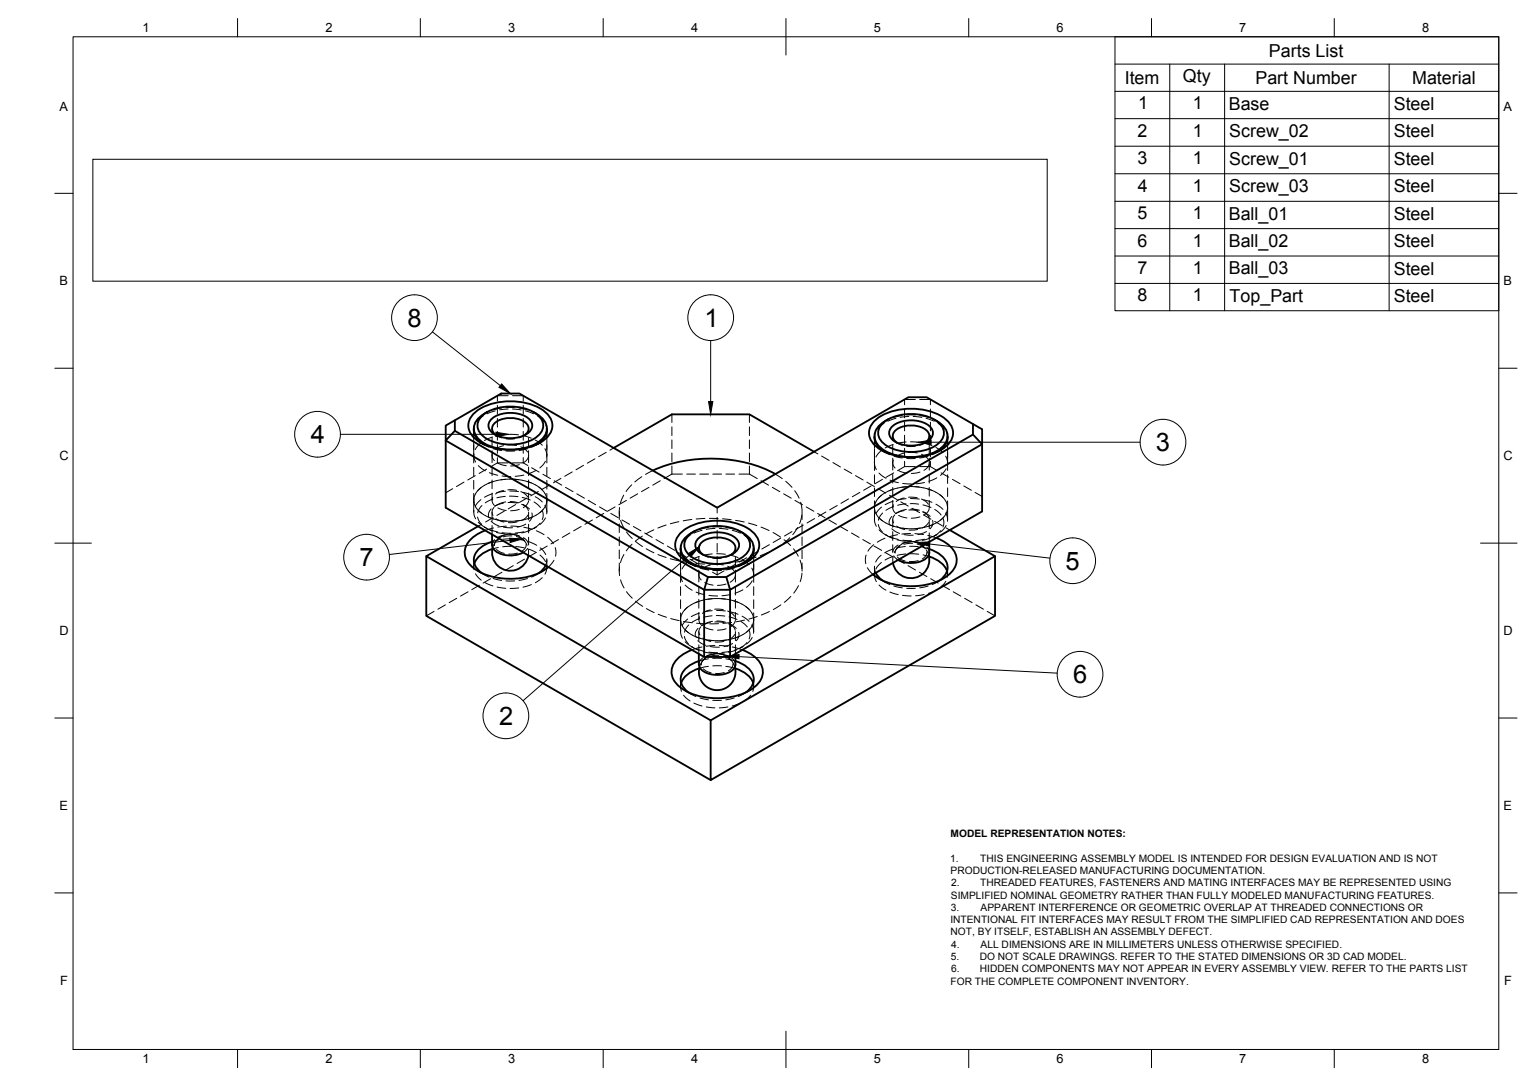
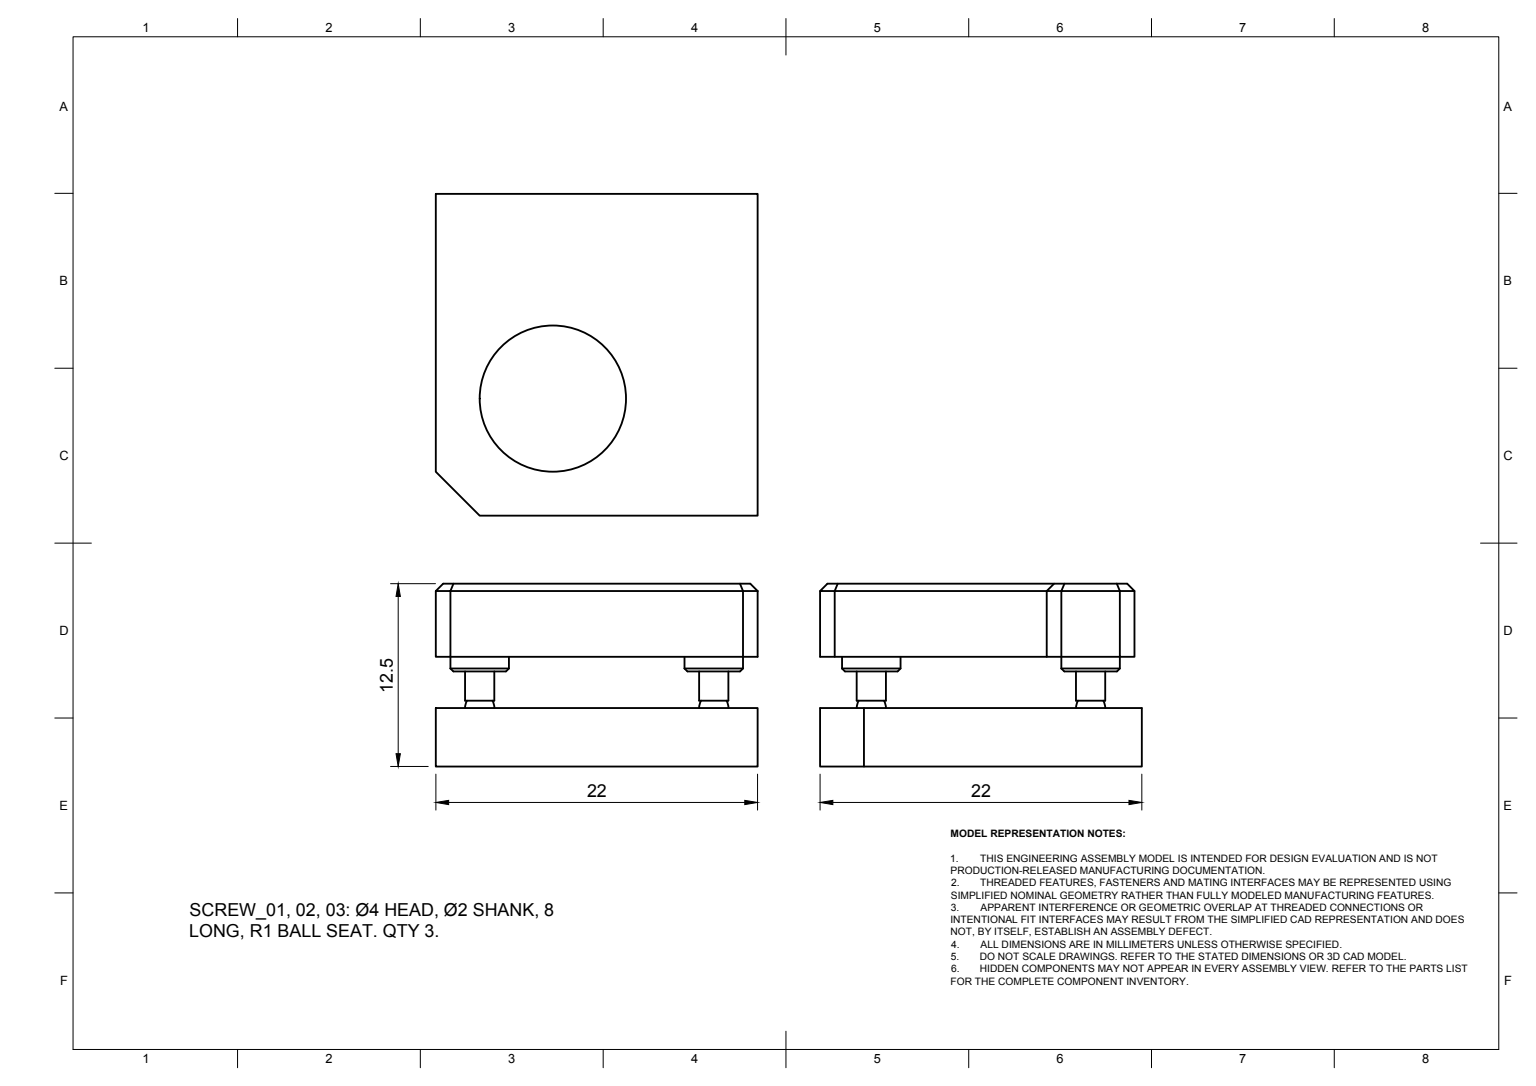
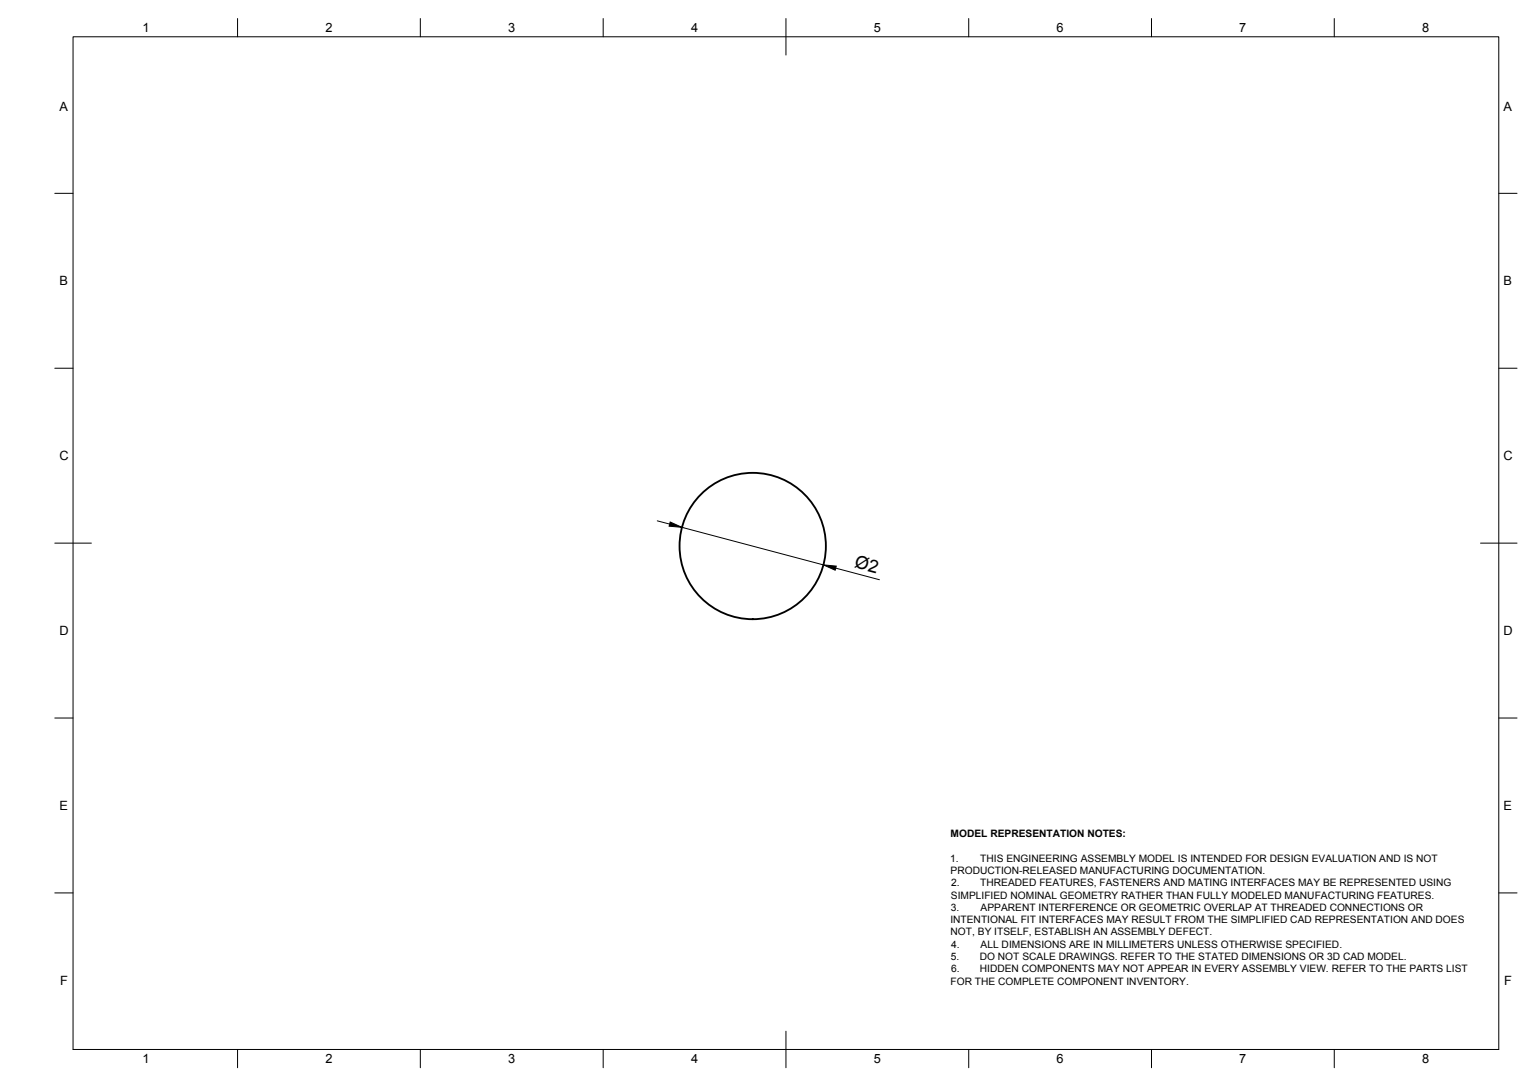
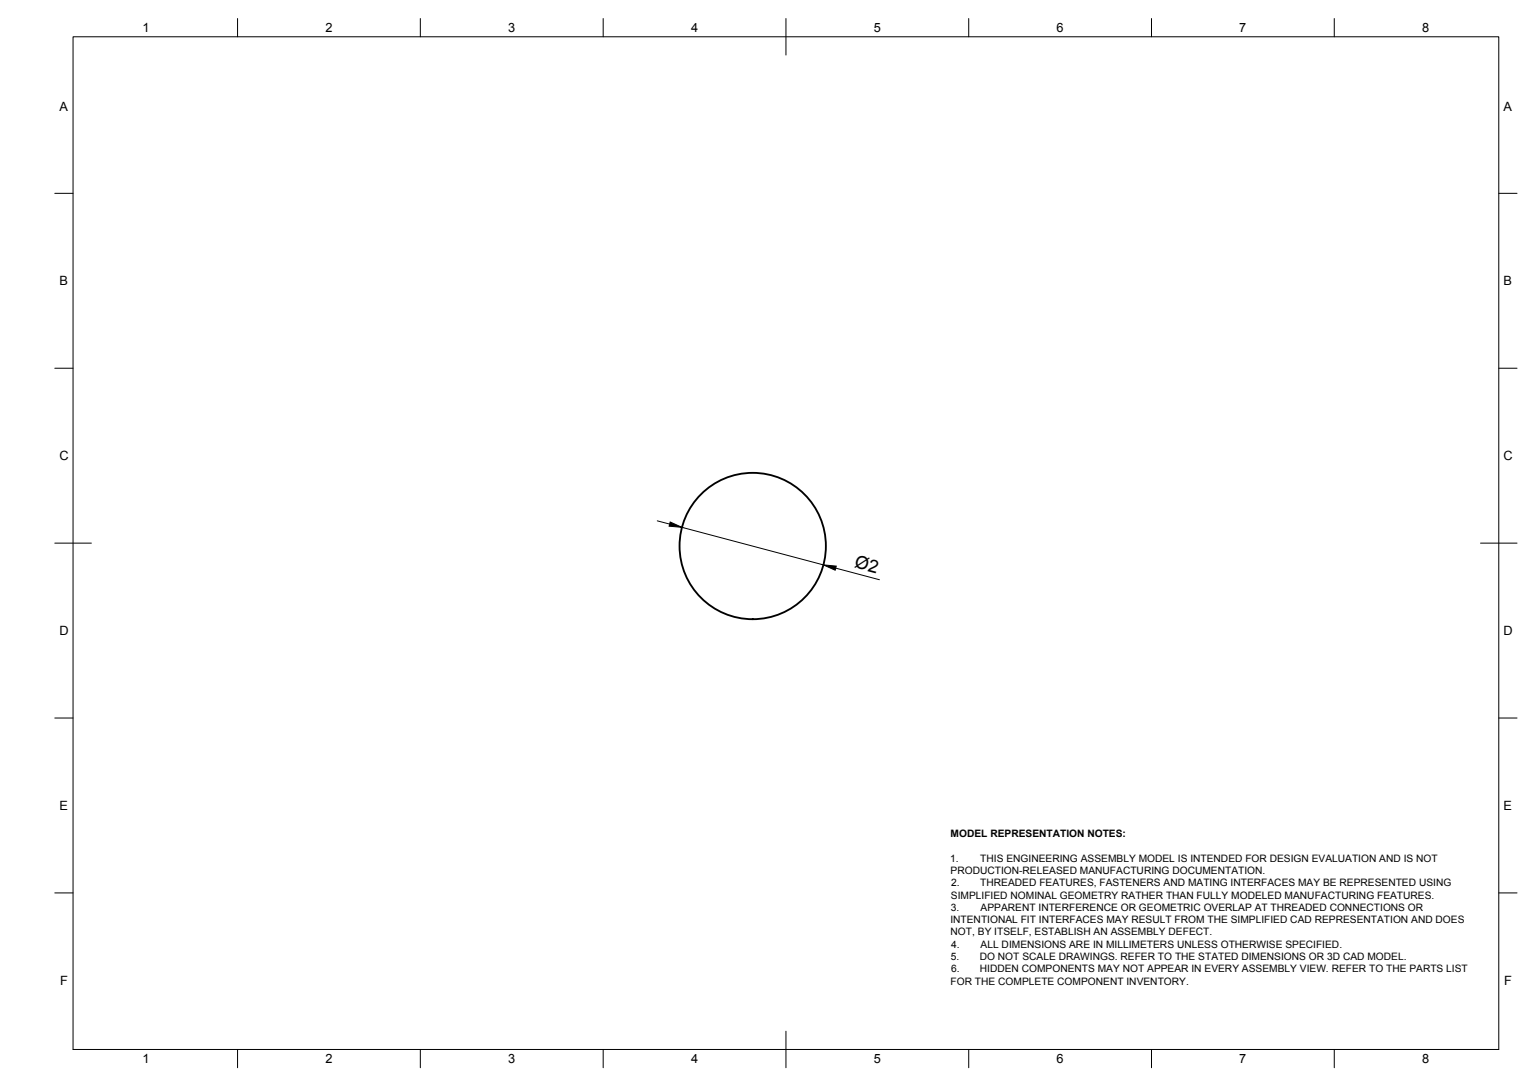
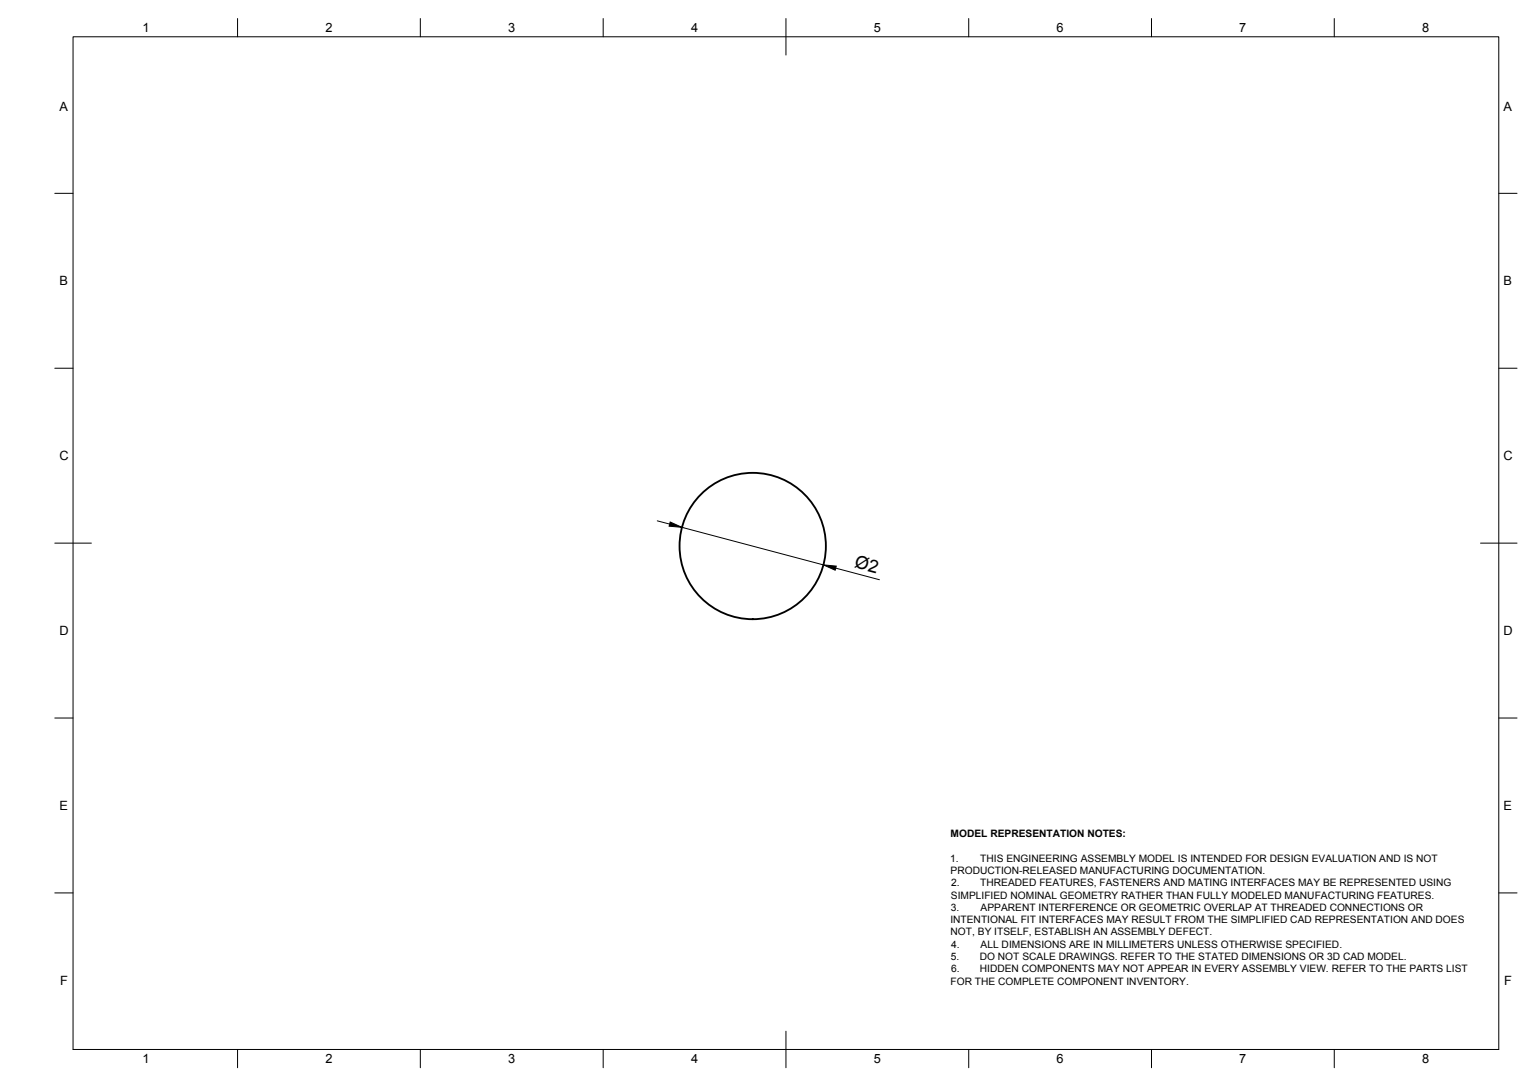
ISO-10303-21;
HEADER;
/* Generated by software containing ST-Developer
 * from STEP Tools, Inc. (www.steptools.com) 
 */

FILE_DESCRIPTION(
/* description */ (''),
/* implementation_level */ '2;1');

FILE_NAME(
/* name */ 'BR-151',
/* time_stamp */ '2026-10-04T23:23:09-07:00',
/* author */ (''),
/* organization */ (''),
/* preprocessor_version */ 'ST-DEVELOPER v20.2',
/* originating_system */ 'Autodesk Translation Framework v15.15.0.0',
/* authorisation */ '');

FILE_SCHEMA (('AUTOMOTIVE_DESIGN { 1 0 10303 214 3 1 1 }'));
ENDSEC;

DATA;
#10=MECHANICAL_DESIGN_GEOMETRIC_PRESENTATION_REPRESENTATION('',(#65,#66,
#67,#68,#69,#70,#71,#72,#73,#74,#75),#2676);
#11=ITEM_DEFINED_TRANSFORMATION($,$,#1577,#1754);
#12=ITEM_DEFINED_TRANSFORMATION($,$,#1606,#1755);
#13=ITEM_DEFINED_TRANSFORMATION($,$,#1639,#1756);
#14=ITEM_DEFINED_TRANSFORMATION($,$,#1672,#1757);
#15=ITEM_DEFINED_TRANSFORMATION($,$,#1705,#1758);
#16=ITEM_DEFINED_TRANSFORMATION($,$,#1708,#1759);
#17=ITEM_DEFINED_TRANSFORMATION($,$,#1711,#1760);
#18=ITEM_DEFINED_TRANSFORMATION($,$,#1714,#1761);
#19=(
REPRESENTATION_RELATIONSHIP($,$,#2708,#2707)
REPRESENTATION_RELATIONSHIP_WITH_TRANSFORMATION(#11)
SHAPE_REPRESENTATION_RELATIONSHIP()
);
#20=(
REPRESENTATION_RELATIONSHIP($,$,#2709,#2707)
REPRESENTATION_RELATIONSHIP_WITH_TRANSFORMATION(#12)
SHAPE_REPRESENTATION_RELATIONSHIP()
);
#21=(
REPRESENTATION_RELATIONSHIP($,$,#2710,#2707)
REPRESENTATION_RELATIONSHIP_WITH_TRANSFORMATION(#13)
SHAPE_REPRESENTATION_RELATIONSHIP()
);
#22=(
REPRESENTATION_RELATIONSHIP($,$,#2711,#2707)
REPRESENTATION_RELATIONSHIP_WITH_TRANSFORMATION(#14)
SHAPE_REPRESENTATION_RELATIONSHIP()
);
#23=(
REPRESENTATION_RELATIONSHIP($,$,#2712,#2707)
REPRESENTATION_RELATIONSHIP_WITH_TRANSFORMATION(#15)
SHAPE_REPRESENTATION_RELATIONSHIP()
);
#24=(
REPRESENTATION_RELATIONSHIP($,$,#2713,#2707)
REPRESENTATION_RELATIONSHIP_WITH_TRANSFORMATION(#16)
SHAPE_REPRESENTATION_RELATIONSHIP()
);
#25=(
REPRESENTATION_RELATIONSHIP($,$,#2714,#2707)
REPRESENTATION_RELATIONSHIP_WITH_TRANSFORMATION(#17)
SHAPE_REPRESENTATION_RELATIONSHIP()
);
#26=(
REPRESENTATION_RELATIONSHIP($,$,#2715,#2707)
REPRESENTATION_RELATIONSHIP_WITH_TRANSFORMATION(#18)
SHAPE_REPRESENTATION_RELATIONSHIP()
);
#27=CONTEXT_DEPENDENT_SHAPE_REPRESENTATION(#19,#2699);
#28=CONTEXT_DEPENDENT_SHAPE_REPRESENTATION(#20,#2700);
#29=CONTEXT_DEPENDENT_SHAPE_REPRESENTATION(#21,#2701);
#30=CONTEXT_DEPENDENT_SHAPE_REPRESENTATION(#22,#2702);
#31=CONTEXT_DEPENDENT_SHAPE_REPRESENTATION(#23,#2703);
#32=CONTEXT_DEPENDENT_SHAPE_REPRESENTATION(#24,#2704);
#33=CONTEXT_DEPENDENT_SHAPE_REPRESENTATION(#25,#2705);
#34=CONTEXT_DEPENDENT_SHAPE_REPRESENTATION(#26,#2706);
#35=NEXT_ASSEMBLY_USAGE_OCCURRENCE('Base:1','Base:1','Base:1',#2717,#2718,
'Base:1');
#36=NEXT_ASSEMBLY_USAGE_OCCURRENCE('Screw_02:1','Screw_02:1',
'Screw_02:1',#2717,#2719,'Screw_02:1');
#37=NEXT_ASSEMBLY_USAGE_OCCURRENCE('Screw_01:1','Screw_01:1',
'Screw_01:1',#2717,#2720,'Screw_01:1');
#38=NEXT_ASSEMBLY_USAGE_OCCURRENCE('Screw_03:1','Screw_03:1',
'Screw_03:1',#2717,#2721,'Screw_03:1');
#39=NEXT_ASSEMBLY_USAGE_OCCURRENCE('Ball_01:1','Ball_01:1','Ball_01:1',
#2717,#2722,'Ball_01:1');
#40=NEXT_ASSEMBLY_USAGE_OCCURRENCE('Ball_02:1','Ball_02:1','Ball_02:1',
#2717,#2723,'Ball_02:1');
#41=NEXT_ASSEMBLY_USAGE_OCCURRENCE('Ball_03:1','Ball_03:1','Ball_03:1',
#2717,#2724,'Ball_03:1');
#42=NEXT_ASSEMBLY_USAGE_OCCURRENCE('Top_part:1','Top_part:1',
'Top_part:1',#2717,#2725,'Top_part:1');
#43=SPHERICAL_SURFACE('',#1637,1.);
#44=SPHERICAL_SURFACE('',#1670,1.);
#45=SPHERICAL_SURFACE('',#1703,1.);
#46=SPHERICAL_SURFACE('',#1706,1.);
#47=SPHERICAL_SURFACE('',#1709,1.);
#48=SPHERICAL_SURFACE('',#1712,1.);
#49=SHAPE_REPRESENTATION_RELATIONSHIP('SRR','None',#2708,#57);
#50=SHAPE_REPRESENTATION_RELATIONSHIP('SRR','None',#2709,#58);
#51=SHAPE_REPRESENTATION_RELATIONSHIP('SRR','None',#2710,#59);
#52=SHAPE_REPRESENTATION_RELATIONSHIP('SRR','None',#2711,#60);
#53=SHAPE_REPRESENTATION_RELATIONSHIP('SRR','None',#2712,#61);
#54=SHAPE_REPRESENTATION_RELATIONSHIP('SRR','None',#2713,#62);
#55=SHAPE_REPRESENTATION_RELATIONSHIP('SRR','None',#2714,#63);
#56=SHAPE_REPRESENTATION_RELATIONSHIP('SRR','None',#2715,#64);
#57=ADVANCED_BREP_SHAPE_REPRESENTATION('',(#76),#2668);
#58=ADVANCED_BREP_SHAPE_REPRESENTATION('',(#77,#78),#2669);
#59=ADVANCED_BREP_SHAPE_REPRESENTATION('',(#79,#80),#2670);
#60=ADVANCED_BREP_SHAPE_REPRESENTATION('',(#81,#82),#2671);
#61=ADVANCED_BREP_SHAPE_REPRESENTATION('',(#83),#2672);
#62=ADVANCED_BREP_SHAPE_REPRESENTATION('',(#84),#2673);
#63=ADVANCED_BREP_SHAPE_REPRESENTATION('',(#85),#2674);
#64=ADVANCED_BREP_SHAPE_REPRESENTATION('',(#86),#2675);
#65=STYLED_ITEM('',(#2757),#76);
#66=STYLED_ITEM('',(#2757),#77);
#67=STYLED_ITEM('',(#2757),#78);
#68=STYLED_ITEM('',(#2757),#79);
#69=STYLED_ITEM('',(#2757),#80);
#70=STYLED_ITEM('',(#2757),#81);
#71=STYLED_ITEM('',(#2757),#82);
#72=STYLED_ITEM('',(#2757),#83);
#73=STYLED_ITEM('',(#2757),#84);
#74=STYLED_ITEM('',(#2757),#85);
#75=STYLED_ITEM('',(#2757),#86);
#76=MANIFOLD_SOLID_BREP('Body1',#1476);
#77=MANIFOLD_SOLID_BREP('Body1',#1477);
#78=MANIFOLD_SOLID_BREP('Body1',#1478);
#79=MANIFOLD_SOLID_BREP('Body1',#1479);
#80=MANIFOLD_SOLID_BREP('Body1',#1480);
#81=MANIFOLD_SOLID_BREP('Body1',#1481);
#82=MANIFOLD_SOLID_BREP('Body1',#1482);
#83=MANIFOLD_SOLID_BREP('Body1',#1483);
#84=MANIFOLD_SOLID_BREP('Body1',#1484);
#85=MANIFOLD_SOLID_BREP('Body1',#1485);
#86=MANIFOLD_SOLID_BREP('Body1',#1486);
#87=CYLINDRICAL_SURFACE('',#1585,2.);
#88=CYLINDRICAL_SURFACE('',#1589,2.);
#89=CYLINDRICAL_SURFACE('',#1593,2.);
#90=CYLINDRICAL_SURFACE('',#1598,5.);
#91=CYLINDRICAL_SURFACE('',#1610,1.);
#92=CYLINDRICAL_SURFACE('',#1614,2.);
#93=CYLINDRICAL_SURFACE('',#1622,1.);
#94=CYLINDRICAL_SURFACE('',#1626,1.);
#95=CYLINDRICAL_SURFACE('',#1630,2.);
#96=CYLINDRICAL_SURFACE('',#1643,1.);
#97=CYLINDRICAL_SURFACE('',#1647,2.);
#98=CYLINDRICAL_SURFACE('',#1655,1.);
#99=CYLINDRICAL_SURFACE('',#1659,1.);
#100=CYLINDRICAL_SURFACE('',#1663,2.);
#101=CYLINDRICAL_SURFACE('',#1676,1.);
#102=CYLINDRICAL_SURFACE('',#1680,2.);
#103=CYLINDRICAL_SURFACE('',#1688,1.);
#104=CYLINDRICAL_SURFACE('',#1692,1.);
#105=CYLINDRICAL_SURFACE('',#1696,2.);
#106=CYLINDRICAL_SURFACE('',#1721,2.);
#107=CYLINDRICAL_SURFACE('',#1725,2.);
#108=CYLINDRICAL_SURFACE('',#1753,2.);
#109=FACE_BOUND('',#287,.T.);
#110=FACE_BOUND('',#288,.T.);
#111=FACE_BOUND('',#289,.T.);
#112=FACE_BOUND('',#290,.T.);
#113=FACE_BOUND('',#306,.T.);
#114=FACE_BOUND('',#308,.T.);
#115=FACE_BOUND('',#313,.T.);
#116=FACE_BOUND('',#316,.T.);
#117=FACE_BOUND('',#321,.T.);
#118=FACE_BOUND('',#325,.T.);
#119=FACE_BOUND('',#329,.T.);
#120=FACE_BOUND('',#334,.T.);
#121=FACE_BOUND('',#337,.T.);
#122=FACE_BOUND('',#342,.T.);
#123=FACE_BOUND('',#346,.T.);
#124=FACE_BOUND('',#350,.T.);
#125=FACE_BOUND('',#355,.T.);
#126=FACE_BOUND('',#358,.T.);
#127=FACE_BOUND('',#363,.T.);
#128=FACE_BOUND('',#367,.T.);
#129=FACE_BOUND('',#375,.T.);
#130=FACE_BOUND('',#376,.T.);
#131=FACE_BOUND('',#377,.T.);
#132=FACE_BOUND('',#390,.T.);
#133=FACE_BOUND('',#391,.T.);
#134=FACE_BOUND('',#392,.T.);
#135=PLANE('',#1581);
#136=PLANE('',#1595);
#137=PLANE('',#1596);
#138=PLANE('',#1597);
#139=PLANE('',#1600);
#140=PLANE('',#1601);
#141=PLANE('',#1602);
#142=PLANE('',#1603);
#143=PLANE('',#1604);
#144=PLANE('',#1605);
#145=PLANE('',#1607);
#146=PLANE('',#1616);
#147=PLANE('',#1619);
#148=PLANE('',#1624);
#149=PLANE('',#1628);
#150=PLANE('',#1634);
#151=PLANE('',#1640);
#152=PLANE('',#1649);
#153=PLANE('',#1652);
#154=PLANE('',#1657);
#155=PLANE('',#1661);
#156=PLANE('',#1667);
#157=PLANE('',#1673);
#158=PLANE('',#1682);
#159=PLANE('',#1685);
#160=PLANE('',#1690);
#161=PLANE('',#1694);
#162=PLANE('',#1700);
#163=PLANE('',#1718);
#164=PLANE('',#1727);
#165=PLANE('',#1728);
#166=PLANE('',#1729);
#167=PLANE('',#1730);
#168=PLANE('',#1731);
#169=PLANE('',#1732);
#170=PLANE('',#1733);
#171=PLANE('',#1734);
#172=PLANE('',#1735);
#173=PLANE('',#1737);
#174=PLANE('',#1738);
#175=PLANE('',#1739);
#176=PLANE('',#1740);
#177=PLANE('',#1741);
#178=PLANE('',#1742);
#179=PLANE('',#1743);
#180=PLANE('',#1744);
#181=PLANE('',#1745);
#182=PLANE('',#1746);
#183=PLANE('',#1747);
#184=PLANE('',#1748);
#185=PLANE('',#1749);
#186=PLANE('',#1750);
#187=FACE_OUTER_BOUND('',#285,.T.);
#188=FACE_OUTER_BOUND('',#286,.T.);
#189=FACE_OUTER_BOUND('',#291,.T.);
#190=FACE_OUTER_BOUND('',#292,.T.);
#191=FACE_OUTER_BOUND('',#293,.T.);
#192=FACE_OUTER_BOUND('',#294,.T.);
#193=FACE_OUTER_BOUND('',#295,.T.);
#194=FACE_OUTER_BOUND('',#296,.T.);
#195=FACE_OUTER_BOUND('',#297,.T.);
#196=FACE_OUTER_BOUND('',#298,.T.);
#197=FACE_OUTER_BOUND('',#299,.T.);
#198=FACE_OUTER_BOUND('',#300,.T.);
#199=FACE_OUTER_BOUND('',#301,.T.);
#200=FACE_OUTER_BOUND('',#302,.T.);
#201=FACE_OUTER_BOUND('',#303,.T.);
#202=FACE_OUTER_BOUND('',#304,.T.);
#203=FACE_OUTER_BOUND('',#305,.T.);
#204=FACE_OUTER_BOUND('',#307,.T.);
#205=FACE_OUTER_BOUND('',#309,.T.);
#206=FACE_OUTER_BOUND('',#310,.T.);
#207=FACE_OUTER_BOUND('',#311,.T.);
#208=FACE_OUTER_BOUND('',#312,.T.);
#209=FACE_OUTER_BOUND('',#314,.T.);
#210=FACE_OUTER_BOUND('',#315,.T.);
#211=FACE_OUTER_BOUND('',#317,.T.);
#212=FACE_OUTER_BOUND('',#318,.T.);
#213=FACE_OUTER_BOUND('',#319,.T.);
#214=FACE_OUTER_BOUND('',#320,.T.);
#215=FACE_OUTER_BOUND('',#322,.T.);
#216=FACE_OUTER_BOUND('',#323,.T.);
#217=FACE_OUTER_BOUND('',#324,.T.);
#218=FACE_OUTER_BOUND('',#326,.T.);
#219=FACE_OUTER_BOUND('',#327,.T.);
#220=FACE_OUTER_BOUND('',#328,.T.);
#221=FACE_OUTER_BOUND('',#330,.T.);
#222=FACE_OUTER_BOUND('',#331,.T.);
#223=FACE_OUTER_BOUND('',#332,.T.);
#224=FACE_OUTER_BOUND('',#333,.T.);
#225=FACE_OUTER_BOUND('',#335,.T.);
#226=FACE_OUTER_BOUND('',#336,.T.);
#227=FACE_OUTER_BOUND('',#338,.T.);
#228=FACE_OUTER_BOUND('',#339,.T.);
#229=FACE_OUTER_BOUND('',#340,.T.);
#230=FACE_OUTER_BOUND('',#341,.T.);
#231=FACE_OUTER_BOUND('',#343,.T.);
#232=FACE_OUTER_BOUND('',#344,.T.);
#233=FACE_OUTER_BOUND('',#345,.T.);
#234=FACE_OUTER_BOUND('',#347,.T.);
#235=FACE_OUTER_BOUND('',#348,.T.);
#236=FACE_OUTER_BOUND('',#349,.T.);
#237=FACE_OUTER_BOUND('',#351,.T.);
#238=FACE_OUTER_BOUND('',#352,.T.);
#239=FACE_OUTER_BOUND('',#353,.T.);
#240=FACE_OUTER_BOUND('',#354,.T.);
#241=FACE_OUTER_BOUND('',#356,.T.);
#242=FACE_OUTER_BOUND('',#357,.T.);
#243=FACE_OUTER_BOUND('',#359,.T.);
#244=FACE_OUTER_BOUND('',#360,.T.);
#245=FACE_OUTER_BOUND('',#361,.T.);
#246=FACE_OUTER_BOUND('',#362,.T.);
#247=FACE_OUTER_BOUND('',#364,.T.);
#248=FACE_OUTER_BOUND('',#365,.T.);
#249=FACE_OUTER_BOUND('',#366,.T.);
#250=FACE_OUTER_BOUND('',#368,.T.);
#251=FACE_OUTER_BOUND('',#369,.T.);
#252=FACE_OUTER_BOUND('',#370,.T.);
#253=FACE_OUTER_BOUND('',#371,.T.);
#254=FACE_OUTER_BOUND('',#372,.T.);
#255=FACE_OUTER_BOUND('',#373,.T.);
#256=FACE_OUTER_BOUND('',#374,.T.);
#257=FACE_OUTER_BOUND('',#378,.T.);
#258=FACE_OUTER_BOUND('',#379,.T.);
#259=FACE_OUTER_BOUND('',#380,.T.);
#260=FACE_OUTER_BOUND('',#381,.T.);
#261=FACE_OUTER_BOUND('',#382,.T.);
#262=FACE_OUTER_BOUND('',#383,.T.);
#263=FACE_OUTER_BOUND('',#384,.T.);
#264=FACE_OUTER_BOUND('',#385,.T.);
#265=FACE_OUTER_BOUND('',#386,.T.);
#266=FACE_OUTER_BOUND('',#387,.T.);
#267=FACE_OUTER_BOUND('',#388,.T.);
#268=FACE_OUTER_BOUND('',#389,.T.);
#269=FACE_OUTER_BOUND('',#393,.T.);
#270=FACE_OUTER_BOUND('',#394,.T.);
#271=FACE_OUTER_BOUND('',#395,.T.);
#272=FACE_OUTER_BOUND('',#396,.T.);
#273=FACE_OUTER_BOUND('',#397,.T.);
#274=FACE_OUTER_BOUND('',#398,.T.);
#275=FACE_OUTER_BOUND('',#399,.T.);
#276=FACE_OUTER_BOUND('',#400,.T.);
#277=FACE_OUTER_BOUND('',#401,.T.);
#278=FACE_OUTER_BOUND('',#402,.T.);
#279=FACE_OUTER_BOUND('',#403,.T.);
#280=FACE_OUTER_BOUND('',#404,.T.);
#281=FACE_OUTER_BOUND('',#405,.T.);
#282=FACE_OUTER_BOUND('',#406,.T.);
#283=FACE_OUTER_BOUND('',#407,.T.);
#284=FACE_OUTER_BOUND('',#408,.T.);
#285=EDGE_LOOP('',(#998,#999,#1000,#1001));
#286=EDGE_LOOP('',(#1002,#1003,#1004,#1005,#1006));
#287=EDGE_LOOP('',(#1007));
#288=EDGE_LOOP('',(#1008));
#289=EDGE_LOOP('',(#1009));
#290=EDGE_LOOP('',(#1010));
#291=EDGE_LOOP('',(#1011,#1012,#1013,#1014));
#292=EDGE_LOOP('',(#1015,#1016,#1017,#1018));
#293=EDGE_LOOP('',(#1019,#1020,#1021,#1022));
#294=EDGE_LOOP('',(#1023,#1024,#1025,#1026));
#295=EDGE_LOOP('',(#1027,#1028,#1029,#1030));
#296=EDGE_LOOP('',(#1031));
#297=EDGE_LOOP('',(#1032));
#298=EDGE_LOOP('',(#1033));
#299=EDGE_LOOP('',(#1034,#1035,#1036,#1037));
#300=EDGE_LOOP('',(#1038,#1039,#1040,#1041));
#301=EDGE_LOOP('',(#1042,#1043,#1044,#1045));
#302=EDGE_LOOP('',(#1046,#1047,#1048,#1049));
#303=EDGE_LOOP('',(#1050,#1051,#1052,#1053));
#304=EDGE_LOOP('',(#1054,#1055,#1056,#1057));
#305=EDGE_LOOP('',(#1058,#1059,#1060,#1061,#1062));
#306=EDGE_LOOP('',(#1063));
#307=EDGE_LOOP('',(#1064));
#308=EDGE_LOOP('',(#1065));
#309=EDGE_LOOP('',(#1066,#1067,#1068,#1069));
#310=EDGE_LOOP('',(#1070,#1071,#1072,#1073));
#311=EDGE_LOOP('',(#1074,#1075,#1076,#1077));
#312=EDGE_LOOP('',(#1078));
#313=EDGE_LOOP('',(#1079));
#314=EDGE_LOOP('',(#1080,#1081,#1082,#1083));
#315=EDGE_LOOP('',(#1084));
#316=EDGE_LOOP('',(#1085));
#317=EDGE_LOOP('',(#1086,#1087,#1088,#1089));
#318=EDGE_LOOP('',(#1090));
#319=EDGE_LOOP('',(#1091,#1092,#1093,#1094));
#320=EDGE_LOOP('',(#1095));
#321=EDGE_LOOP('',(#1096));
#322=EDGE_LOOP('',(#1097,#1098,#1099,#1100));
#323=EDGE_LOOP('',(#1101,#1102,#1103,#1104));
#324=EDGE_LOOP('',(#1105));
#325=EDGE_LOOP('',(#1106));
#326=EDGE_LOOP('',(#1107,#1108,#1109,#1110));
#327=EDGE_LOOP('',(#1111,#1112,#1113));
#328=EDGE_LOOP('',(#1114));
#329=EDGE_LOOP('',(#1115));
#330=EDGE_LOOP('',(#1116,#1117,#1118,#1119));
#331=EDGE_LOOP('',(#1120,#1121,#1122,#1123));
#332=EDGE_LOOP('',(#1124,#1125,#1126,#1127));
#333=EDGE_LOOP('',(#1128));
#334=EDGE_LOOP('',(#1129));
#335=EDGE_LOOP('',(#1130,#1131,#1132,#1133));
#336=EDGE_LOOP('',(#1134));
#337=EDGE_LOOP('',(#1135));
#338=EDGE_LOOP('',(#1136,#1137,#1138,#1139));
#339=EDGE_LOOP('',(#1140));
#340=EDGE_LOOP('',(#1141,#1142,#1143,#1144));
#341=EDGE_LOOP('',(#1145));
#342=EDGE_LOOP('',(#1146));
#343=EDGE_LOOP('',(#1147,#1148,#1149,#1150));
#344=EDGE_LOOP('',(#1151,#1152,#1153,#1154));
#345=EDGE_LOOP('',(#1155));
#346=EDGE_LOOP('',(#1156));
#347=EDGE_LOOP('',(#1157,#1158,#1159,#1160));
#348=EDGE_LOOP('',(#1161,#1162,#1163));
#349=EDGE_LOOP('',(#1164));
#350=EDGE_LOOP('',(#1165));
#351=EDGE_LOOP('',(#1166,#1167,#1168,#1169));
#352=EDGE_LOOP('',(#1170,#1171,#1172,#1173));
#353=EDGE_LOOP('',(#1174,#1175,#1176,#1177));
#354=EDGE_LOOP('',(#1178));
#355=EDGE_LOOP('',(#1179));
#356=EDGE_LOOP('',(#1180,#1181,#1182,#1183));
#357=EDGE_LOOP('',(#1184));
#358=EDGE_LOOP('',(#1185));
#359=EDGE_LOOP('',(#1186,#1187,#1188,#1189));
#360=EDGE_LOOP('',(#1190));
#361=EDGE_LOOP('',(#1191,#1192,#1193,#1194));
#362=EDGE_LOOP('',(#1195));
#363=EDGE_LOOP('',(#1196));
#364=EDGE_LOOP('',(#1197,#1198,#1199,#1200));
#365=EDGE_LOOP('',(#1201,#1202,#1203,#1204));
#366=EDGE_LOOP('',(#1205));
#367=EDGE_LOOP('',(#1206));
#368=EDGE_LOOP('',(#1207,#1208,#1209,#1210));
#369=EDGE_LOOP('',(#1211,#1212,#1213));
#370=EDGE_LOOP('',(#1214,#1215));
#371=EDGE_LOOP('',(#1216,#1217));
#372=EDGE_LOOP('',(#1218,#1219));
#373=EDGE_LOOP('',(#1220,#1221,#1222,#1223));
#374=EDGE_LOOP('',(#1224,#1225,#1226,#1227,#1228,#1229,#1230,#1231,#1232,
#1233,#1234));
#375=EDGE_LOOP('',(#1235));
#376=EDGE_LOOP('',(#1236));
#377=EDGE_LOOP('',(#1237));
#378=EDGE_LOOP('',(#1238,#1239,#1240,#1241));
#379=EDGE_LOOP('',(#1242,#1243,#1244,#1245));
#380=EDGE_LOOP('',(#1246,#1247,#1248,#1249));
#381=EDGE_LOOP('',(#1250,#1251,#1252,#1253));
#382=EDGE_LOOP('',(#1254,#1255,#1256,#1257));
#383=EDGE_LOOP('',(#1258,#1259,#1260,#1261));
#384=EDGE_LOOP('',(#1262,#1263,#1264,#1265));
#385=EDGE_LOOP('',(#1266,#1267,#1268,#1269));
#386=EDGE_LOOP('',(#1270,#1271,#1272,#1273));
#387=EDGE_LOOP('',(#1274,#1275,#1276,#1277));
#388=EDGE_LOOP('',(#1278,#1279,#1280,#1281));
#389=EDGE_LOOP('',(#1282,#1283,#1284,#1285,#1286,#1287,#1288,#1289,#1290,
#1291,#1292));
#390=EDGE_LOOP('',(#1293));
#391=EDGE_LOOP('',(#1294));
#392=EDGE_LOOP('',(#1295));
#393=EDGE_LOOP('',(#1296,#1297,#1298,#1299));
#394=EDGE_LOOP('',(#1300,#1301,#1302,#1303));
#395=EDGE_LOOP('',(#1304,#1305,#1306,#1307));
#396=EDGE_LOOP('',(#1308,#1309,#1310,#1311));
#397=EDGE_LOOP('',(#1312,#1313,#1314,#1315));
#398=EDGE_LOOP('',(#1316,#1317,#1318,#1319));
#399=EDGE_LOOP('',(#1320,#1321,#1322,#1323));
#400=EDGE_LOOP('',(#1324,#1325,#1326,#1327));
#401=EDGE_LOOP('',(#1328,#1329,#1330,#1331));
#402=EDGE_LOOP('',(#1332,#1333,#1334,#1335));
#403=EDGE_LOOP('',(#1336,#1337,#1338,#1339));
#404=EDGE_LOOP('',(#1340,#1341,#1342,#1343));
#405=EDGE_LOOP('',(#1344,#1345,#1346,#1347));
#406=EDGE_LOOP('',(#1348,#1349,#1350,#1351));
#407=EDGE_LOOP('',(#1352,#1353,#1354,#1355));
#408=EDGE_LOOP('',(#1356,#1357,#1358,#1359));
#409=LINE('',#2250,#519);
#410=LINE('',#2255,#520);
#411=LINE('',#2257,#521);
#412=LINE('',#2259,#522);
#413=LINE('',#2261,#523);
#414=LINE('',#2262,#524);
#415=LINE('',#2271,#525);
#416=LINE('',#2276,#526);
#417=LINE('',#2279,#527);
#418=LINE('',#2284,#528);
#419=LINE('',#2287,#529);
#420=LINE('',#2295,#530);
#421=LINE('',#2299,#531);
#422=LINE('',#2300,#532);
#423=LINE('',#2301,#533);
#424=LINE('',#2304,#534);
#425=LINE('',#2305,#535);
#426=LINE('',#2308,#536);
#427=LINE('',#2309,#537);
#428=LINE('',#2312,#538);
#429=LINE('',#2313,#539);
#430=LINE('',#2315,#540);
#431=LINE('',#2326,#541);
#432=LINE('',#2329,#542);
#433=LINE('',#2333,#543);
#434=LINE('',#2339,#544);
#435=LINE('',#2347,#545);
#436=LINE('',#2355,#546);
#437=LINE('',#2362,#547);
#438=LINE('',#2365,#548);
#439=LINE('',#2371,#549);
#440=LINE('',#2384,#550);
#441=LINE('',#2387,#551);
#442=LINE('',#2391,#552);
#443=LINE('',#2397,#553);
#444=LINE('',#2405,#554);
#445=LINE('',#2413,#555);
#446=LINE('',#2420,#556);
#447=LINE('',#2423,#557);
#448=LINE('',#2429,#558);
#449=LINE('',#2442,#559);
#450=LINE('',#2445,#560);
#451=LINE('',#2449,#561);
#452=LINE('',#2455,#562);
#453=LINE('',#2463,#563);
#454=LINE('',#2471,#564);
#455=LINE('',#2478,#565);
#456=LINE('',#2481,#566);
#457=LINE('',#2487,#567);
#458=LINE('',#2511,#568);
#459=LINE('',#2516,#569);
#460=LINE('',#2518,#570);
#461=LINE('',#2520,#571);
#462=LINE('',#2522,#572);
#463=LINE('',#2524,#573);
#464=LINE('',#2526,#574);
#465=LINE('',#2528,#575);
#466=LINE('',#2530,#576);
#467=LINE('',#2532,#577);
#468=LINE('',#2534,#578);
#469=LINE('',#2535,#579);
#470=LINE('',#2542,#580);
#471=LINE('',#2547,#581);
#472=LINE('',#2550,#582);
#473=LINE('',#2555,#583);
#474=LINE('',#2556,#584);
#475=LINE('',#2557,#585);
#476=LINE('',#2560,#586);
#477=LINE('',#2561,#587);
#478=LINE('',#2564,#588);
#479=LINE('',#2565,#589);
#480=LINE('',#2568,#590);
#481=LINE('',#2569,#591);
#482=LINE('',#2572,#592);
#483=LINE('',#2574,#593);
#484=LINE('',#2575,#594);
#485=LINE('',#2578,#595);
#486=LINE('',#2579,#596);
#487=LINE('',#2582,#597);
#488=LINE('',#2583,#598);
#489=LINE('',#2586,#599);
#490=LINE('',#2587,#600);
#491=LINE('',#2590,#601);
#492=LINE('',#2592,#602);
#493=LINE('',#2594,#603);
#494=LINE('',#2596,#604);
#495=LINE('',#2598,#605);
#496=LINE('',#2600,#606);
#497=LINE('',#2601,#607);
#498=LINE('',#2606,#608);
#499=LINE('',#2607,#609);
#500=LINE('',#2610,#610);
#501=LINE('',#2612,#611);
#502=LINE('',#2613,#612);
#503=LINE('',#2616,#613);
#504=LINE('',#2617,#614);
#505=LINE('',#2620,#615);
#506=LINE('',#2621,#616);
#507=LINE('',#2624,#617);
#508=LINE('',#2625,#618);
#509=LINE('',#2627,#619);
#510=LINE('',#2629,#620);
#511=LINE('',#2631,#621);
#512=LINE('',#2633,#622);
#513=LINE('',#2635,#623);
#514=LINE('',#2637,#624);
#515=LINE('',#2639,#625);
#516=LINE('',#2641,#626);
#517=LINE('',#2646,#627);
#518=LINE('',#2648,#628);
#519=VECTOR('',#1770,2.25);
#520=VECTOR('',#1775,10.);
#521=VECTOR('',#1776,10.);
#522=VECTOR('',#1777,10.);
#523=VECTOR('',#1778,10.);
#524=VECTOR('',#1779,10.);
#525=VECTOR('',#1788,2.);
#526=VECTOR('',#1795,2.25);
#527=VECTOR('',#1798,2.);
#528=VECTOR('',#1805,2.25);
#529=VECTOR('',#1808,2.);
#530=VECTOR('',#1821,5.);
#531=VECTOR('',#1824,10.);
#532=VECTOR('',#1825,10.);
#533=VECTOR('',#1826,10.);
#534=VECTOR('',#1829,10.);
#535=VECTOR('',#1830,10.);
#536=VECTOR('',#1833,10.);
#537=VECTOR('',#1834,10.);
#538=VECTOR('',#1837,10.);
#539=VECTOR('',#1838,10.);
#540=VECTOR('',#1841,10.);
#541=VECTOR('',#1856,1.);
#542=VECTOR('',#1859,1.1);
#543=VECTOR('',#1864,2.);
#544=VECTOR('',#1873,1.9);
#545=VECTOR('',#1882,1.);
#546=VECTOR('',#1893,1.);
#547=VECTOR('',#1902,2.);
#548=VECTOR('',#1905,1.9);
#549=VECTOR('',#1914,1.1);
#550=VECTOR('',#1931,1.);
#551=VECTOR('',#1934,1.1);
#552=VECTOR('',#1939,2.);
#553=VECTOR('',#1948,1.9);
#554=VECTOR('',#1957,1.);
#555=VECTOR('',#1968,1.);
#556=VECTOR('',#1977,2.);
#557=VECTOR('',#1980,1.9);
#558=VECTOR('',#1989,1.1);
#559=VECTOR('',#2006,1.);
#560=VECTOR('',#2009,1.1);
#561=VECTOR('',#2014,2.);
#562=VECTOR('',#2023,1.9);
#563=VECTOR('',#2032,1.);
#564=VECTOR('',#2043,1.);
#565=VECTOR('',#2052,2.);
#566=VECTOR('',#2055,1.9);
#567=VECTOR('',#2064,1.1);
#568=VECTOR('',#2093,2.15);
#569=VECTOR('',#2098,10.);
#570=VECTOR('',#2099,10.);
#571=VECTOR('',#2100,10.);
#572=VECTOR('',#2101,10.);
#573=VECTOR('',#2102,10.);
#574=VECTOR('',#2103,10.);
#575=VECTOR('',#2104,10.);
#576=VECTOR('',#2105,10.);
#577=VECTOR('',#2106,10.);
#578=VECTOR('',#2107,9.99999999999999);
#579=VECTOR('',#2108,10.);
#580=VECTOR('',#2115,2.);
#581=VECTOR('',#2122,2.15);
#582=VECTOR('',#2125,2.);
#583=VECTOR('',#2130,10.);
#584=VECTOR('',#2131,10.);
#585=VECTOR('',#2132,10.);
#586=VECTOR('',#2135,10.);
#587=VECTOR('',#2136,10.);
#588=VECTOR('',#2139,10.);
#589=VECTOR('',#2140,9.99999999999999);
#590=VECTOR('',#2143,10.);
#591=VECTOR('',#2144,10.);
#592=VECTOR('',#2147,10.);
#593=VECTOR('',#2148,10.);
#594=VECTOR('',#2149,10.);
#595=VECTOR('',#2152,10.);
#596=VECTOR('',#2153,10.);
#597=VECTOR('',#2156,10.);
#598=VECTOR('',#2157,9.99999999999999);
#599=VECTOR('',#2160,10.);
#600=VECTOR('',#2161,10.);
#601=VECTOR('',#2164,10.);
#602=VECTOR('',#2165,10.);
#603=VECTOR('',#2166,10.);
#604=VECTOR('',#2167,10.);
#605=VECTOR('',#2168,10.);
#606=VECTOR('',#2169,10.);
#607=VECTOR('',#2170,10.);
#608=VECTOR('',#2175,10.);
#609=VECTOR('',#2176,10.);
#610=VECTOR('',#2179,10.);
#611=VECTOR('',#2180,10.);
#612=VECTOR('',#2181,10.);
#613=VECTOR('',#2184,10.);
#614=VECTOR('',#2185,10.);
#615=VECTOR('',#2188,10.);
#616=VECTOR('',#2189,10.);
#617=VECTOR('',#2192,10.);
#618=VECTOR('',#2193,10.);
#619=VECTOR('',#2196,10.);
#620=VECTOR('',#2199,10.);
#621=VECTOR('',#2202,10.);
#622=VECTOR('',#2205,10.);
#623=VECTOR('',#2208,10.);
#624=VECTOR('',#2211,10.);
#625=VECTOR('',#2214,10.);
#626=VECTOR('',#2217,10.);
#627=VECTOR('',#2224,2.15);
#628=VECTOR('',#2227,2.);
#629=CIRCLE('',#1579,2.);
#630=CIRCLE('',#1580,2.5);
#631=CIRCLE('',#1582,2.5);
#632=CIRCLE('',#1583,5.);
#633=CIRCLE('',#1584,2.5);
#634=CIRCLE('',#1586,2.);
#635=CIRCLE('',#1588,2.);
#636=CIRCLE('',#1590,2.);
#637=CIRCLE('',#1592,2.);
#638=CIRCLE('',#1594,2.);
#639=CIRCLE('',#1599,5.);
#640=CIRCLE('',#1608,2.);
#641=CIRCLE('',#1609,1.);
#642=CIRCLE('',#1611,1.);
#643=CIRCLE('',#1613,1.2);
#644=CIRCLE('',#1615,2.);
#645=CIRCLE('',#1617,1.8);
#646=CIRCLE('',#1620,1.);
#647=CIRCLE('',#1621,0.866025403784439);
#648=CIRCLE('',#1623,1.);
#649=CIRCLE('',#1625,1.);
#650=CIRCLE('',#1627,1.);
#651=CIRCLE('',#1629,2.);
#652=CIRCLE('',#1631,2.);
#653=CIRCLE('',#1633,1.8);
#654=CIRCLE('',#1635,1.2);
#655=CIRCLE('',#1638,1.);
#656=CIRCLE('',#1641,2.);
#657=CIRCLE('',#1642,1.);
#658=CIRCLE('',#1644,1.);
#659=CIRCLE('',#1646,1.2);
#660=CIRCLE('',#1648,2.);
#661=CIRCLE('',#1650,1.8);
#662=CIRCLE('',#1653,1.);
#663=CIRCLE('',#1654,0.866025403784439);
#664=CIRCLE('',#1656,1.);
#665=CIRCLE('',#1658,1.);
#666=CIRCLE('',#1660,1.);
#667=CIRCLE('',#1662,2.);
#668=CIRCLE('',#1664,2.);
#669=CIRCLE('',#1666,1.8);
#670=CIRCLE('',#1668,1.2);
#671=CIRCLE('',#1671,1.);
#672=CIRCLE('',#1674,2.);
#673=CIRCLE('',#1675,1.);
#674=CIRCLE('',#1677,1.);
#675=CIRCLE('',#1679,1.2);
#676=CIRCLE('',#1681,2.);
#677=CIRCLE('',#1683,1.8);
#678=CIRCLE('',#1686,1.);
#679=CIRCLE('',#1687,0.866025403784439);
#680=CIRCLE('',#1689,1.);
#681=CIRCLE('',#1691,1.);
#682=CIRCLE('',#1693,1.);
#683=CIRCLE('',#1695,2.);
#684=CIRCLE('',#1697,2.);
#685=CIRCLE('',#1699,1.8);
#686=CIRCLE('',#1701,1.2);
#687=CIRCLE('',#1704,1.);
#688=CIRCLE('',#1707,1.);
#689=CIRCLE('',#1710,1.);
#690=CIRCLE('',#1713,1.);
#691=CIRCLE('',#1716,2.);
#692=CIRCLE('',#1717,2.3);
#693=CIRCLE('',#1719,2.3);
#694=CIRCLE('',#1720,2.3);
#695=CIRCLE('',#1722,2.);
#696=CIRCLE('',#1724,2.);
#697=CIRCLE('',#1726,2.);
#698=CIRCLE('',#1736,2.);
#699=CIRCLE('',#1752,2.);
#700=VERTEX_POINT('',#2247);
#701=VERTEX_POINT('',#2249);
#702=VERTEX_POINT('',#2253);
#703=VERTEX_POINT('',#2254);
#704=VERTEX_POINT('',#2256);
#705=VERTEX_POINT('',#2258);
#706=VERTEX_POINT('',#2260);
#707=VERTEX_POINT('',#2263);
#708=VERTEX_POINT('',#2265);
#709=VERTEX_POINT('',#2267);
#710=VERTEX_POINT('',#2270);
#711=VERTEX_POINT('',#2274);
#712=VERTEX_POINT('',#2278);
#713=VERTEX_POINT('',#2282);
#714=VERTEX_POINT('',#2286);
#715=VERTEX_POINT('',#2293);
#716=VERTEX_POINT('',#2297);
#717=VERTEX_POINT('',#2298);
#718=VERTEX_POINT('',#2303);
#719=VERTEX_POINT('',#2307);
#720=VERTEX_POINT('',#2311);
#721=VERTEX_POINT('',#2319);
#722=VERTEX_POINT('',#2321);
#723=VERTEX_POINT('',#2324);
#724=VERTEX_POINT('',#2328);
#725=VERTEX_POINT('',#2332);
#726=VERTEX_POINT('',#2336);
#727=VERTEX_POINT('',#2341);
#728=VERTEX_POINT('',#2343);
#729=VERTEX_POINT('',#2346);
#730=VERTEX_POINT('',#2350);
#731=VERTEX_POINT('',#2353);
#732=VERTEX_POINT('',#2357);
#733=VERTEX_POINT('',#2360);
#734=VERTEX_POINT('',#2364);
#735=VERTEX_POINT('',#2368);
#736=VERTEX_POINT('',#2373);
#737=VERTEX_POINT('',#2377);
#738=VERTEX_POINT('',#2379);
#739=VERTEX_POINT('',#2382);
#740=VERTEX_POINT('',#2386);
#741=VERTEX_POINT('',#2390);
#742=VERTEX_POINT('',#2394);
#743=VERTEX_POINT('',#2399);
#744=VERTEX_POINT('',#2401);
#745=VERTEX_POINT('',#2404);
#746=VERTEX_POINT('',#2408);
#747=VERTEX_POINT('',#2411);
#748=VERTEX_POINT('',#2415);
#749=VERTEX_POINT('',#2418);
#750=VERTEX_POINT('',#2422);
#751=VERTEX_POINT('',#2426);
#752=VERTEX_POINT('',#2431);
#753=VERTEX_POINT('',#2435);
#754=VERTEX_POINT('',#2437);
#755=VERTEX_POINT('',#2440);
#756=VERTEX_POINT('',#2444);
#757=VERTEX_POINT('',#2448);
#758=VERTEX_POINT('',#2452);
#759=VERTEX_POINT('',#2457);
#760=VERTEX_POINT('',#2459);
#761=VERTEX_POINT('',#2462);
#762=VERTEX_POINT('',#2466);
#763=VERTEX_POINT('',#2469);
#764=VERTEX_POINT('',#2473);
#765=VERTEX_POINT('',#2476);
#766=VERTEX_POINT('',#2480);
#767=VERTEX_POINT('',#2484);
#768=VERTEX_POINT('',#2489);
#769=VERTEX_POINT('',#2493);
#770=VERTEX_POINT('',#2494);
#771=VERTEX_POINT('',#2498);
#772=VERTEX_POINT('',#2499);
#773=VERTEX_POINT('',#2503);
#774=VERTEX_POINT('',#2504);
#775=VERTEX_POINT('',#2508);
#776=VERTEX_POINT('',#2510);
#777=VERTEX_POINT('',#2514);
#778=VERTEX_POINT('',#2515);
#779=VERTEX_POINT('',#2517);
#780=VERTEX_POINT('',#2519);
#781=VERTEX_POINT('',#2521);
#782=VERTEX_POINT('',#2523);
#783=VERTEX_POINT('',#2525);
#784=VERTEX_POINT('',#2527);
#785=VERTEX_POINT('',#2529);
#786=VERTEX_POINT('',#2531);
#787=VERTEX_POINT('',#2533);
#788=VERTEX_POINT('',#2536);
#789=VERTEX_POINT('',#2538);
#790=VERTEX_POINT('',#2541);
#791=VERTEX_POINT('',#2545);
#792=VERTEX_POINT('',#2549);
#793=VERTEX_POINT('',#2553);
#794=VERTEX_POINT('',#2554);
#795=VERTEX_POINT('',#2559);
#796=VERTEX_POINT('',#2563);
#797=VERTEX_POINT('',#2567);
#798=VERTEX_POINT('',#2571);
#799=VERTEX_POINT('',#2573);
#800=VERTEX_POINT('',#2577);
#801=VERTEX_POINT('',#2581);
#802=VERTEX_POINT('',#2585);
#803=VERTEX_POINT('',#2589);
#804=VERTEX_POINT('',#2591);
#805=VERTEX_POINT('',#2593);
#806=VERTEX_POINT('',#2595);
#807=VERTEX_POINT('',#2597);
#808=VERTEX_POINT('',#2599);
#809=VERTEX_POINT('',#2602);
#810=VERTEX_POINT('',#2605);
#811=VERTEX_POINT('',#2609);
#812=VERTEX_POINT('',#2611);
#813=VERTEX_POINT('',#2615);
#814=VERTEX_POINT('',#2619);
#815=VERTEX_POINT('',#2623);
#816=VERTEX_POINT('',#2644);
#817=EDGE_CURVE('',#700,#700,#629,.T.);
#818=EDGE_CURVE('',#700,#701,#409,.T.);
#819=EDGE_CURVE('',#701,#701,#630,.T.);
#820=EDGE_CURVE('',#702,#703,#410,.T.);
#821=EDGE_CURVE('',#703,#704,#411,.T.);
#822=EDGE_CURVE('',#704,#705,#412,.T.);
#823=EDGE_CURVE('',#705,#706,#413,.T.);
#824=EDGE_CURVE('',#706,#702,#414,.T.);
#825=EDGE_CURVE('',#707,#707,#631,.T.);
#826=EDGE_CURVE('',#708,#708,#632,.T.);
#827=EDGE_CURVE('',#709,#709,#633,.T.);
#828=EDGE_CURVE('',#700,#710,#415,.T.);
#829=EDGE_CURVE('',#710,#710,#634,.T.);
#830=EDGE_CURVE('',#711,#711,#635,.T.);
#831=EDGE_CURVE('',#711,#707,#416,.T.);
#832=EDGE_CURVE('',#711,#712,#417,.T.);
#833=EDGE_CURVE('',#712,#712,#636,.T.);
#834=EDGE_CURVE('',#713,#713,#637,.T.);
#835=EDGE_CURVE('',#713,#709,#418,.T.);
#836=EDGE_CURVE('',#713,#714,#419,.T.);
#837=EDGE_CURVE('',#714,#714,#638,.T.);
#838=EDGE_CURVE('',#715,#715,#639,.T.);
#839=EDGE_CURVE('',#715,#708,#420,.T.);
#840=EDGE_CURVE('',#716,#717,#421,.T.);
#841=EDGE_CURVE('',#716,#702,#422,.T.);
#842=EDGE_CURVE('',#717,#706,#423,.T.);
#843=EDGE_CURVE('',#718,#717,#424,.T.);
#844=EDGE_CURVE('',#718,#705,#425,.T.);
#845=EDGE_CURVE('',#719,#718,#426,.T.);
#846=EDGE_CURVE('',#719,#704,#427,.T.);
#847=EDGE_CURVE('',#720,#719,#428,.T.);
#848=EDGE_CURVE('',#720,#703,#429,.T.);
#849=EDGE_CURVE('',#716,#720,#430,.T.);
#850=EDGE_CURVE('',#721,#721,#640,.T.);
#851=EDGE_CURVE('',#722,#722,#641,.T.);
#852=EDGE_CURVE('',#723,#723,#642,.T.);
#853=EDGE_CURVE('',#723,#722,#431,.T.);
#854=EDGE_CURVE('',#723,#724,#432,.T.);
#855=EDGE_CURVE('',#724,#724,#643,.T.);
#856=EDGE_CURVE('',#721,#725,#433,.T.);
#857=EDGE_CURVE('',#725,#725,#644,.T.);
#858=EDGE_CURVE('',#726,#726,#645,.T.);
#859=EDGE_CURVE('',#725,#726,#434,.T.);
#860=EDGE_CURVE('',#727,#727,#646,.T.);
#861=EDGE_CURVE('',#728,#728,#647,.T.);
#862=EDGE_CURVE('',#727,#729,#435,.T.);
#863=EDGE_CURVE('',#729,#729,#648,.T.);
#864=EDGE_CURVE('',#730,#730,#649,.T.);
#865=EDGE_CURVE('',#731,#731,#650,.T.);
#866=EDGE_CURVE('',#731,#730,#436,.T.);
#867=EDGE_CURVE('',#732,#732,#651,.T.);
#868=EDGE_CURVE('',#733,#733,#652,.T.);
#869=EDGE_CURVE('',#733,#732,#437,.T.);
#870=EDGE_CURVE('',#733,#734,#438,.T.);
#871=EDGE_CURVE('',#734,#734,#653,.T.);
#872=EDGE_CURVE('',#735,#735,#654,.T.);
#873=EDGE_CURVE('',#729,#735,#439,.T.);
#874=EDGE_CURVE('',#728,#736,#655,.T.);
#875=EDGE_CURVE('',#737,#737,#656,.T.);
#876=EDGE_CURVE('',#738,#738,#657,.T.);
#877=EDGE_CURVE('',#739,#739,#658,.T.);
#878=EDGE_CURVE('',#739,#738,#440,.T.);
#879=EDGE_CURVE('',#739,#740,#441,.T.);
#880=EDGE_CURVE('',#740,#740,#659,.T.);
#881=EDGE_CURVE('',#737,#741,#442,.T.);
#882=EDGE_CURVE('',#741,#741,#660,.T.);
#883=EDGE_CURVE('',#742,#742,#661,.T.);
#884=EDGE_CURVE('',#741,#742,#443,.T.);
#885=EDGE_CURVE('',#743,#743,#662,.T.);
#886=EDGE_CURVE('',#744,#744,#663,.T.);
#887=EDGE_CURVE('',#743,#745,#444,.T.);
#888=EDGE_CURVE('',#745,#745,#664,.T.);
#889=EDGE_CURVE('',#746,#746,#665,.T.);
#890=EDGE_CURVE('',#747,#747,#666,.T.);
#891=EDGE_CURVE('',#747,#746,#445,.T.);
#892=EDGE_CURVE('',#748,#748,#667,.T.);
#893=EDGE_CURVE('',#749,#749,#668,.T.);
#894=EDGE_CURVE('',#749,#748,#446,.T.);
#895=EDGE_CURVE('',#749,#750,#447,.T.);
#896=EDGE_CURVE('',#750,#750,#669,.T.);
#897=EDGE_CURVE('',#751,#751,#670,.T.);
#898=EDGE_CURVE('',#745,#751,#448,.T.);
#899=EDGE_CURVE('',#744,#752,#671,.T.);
#900=EDGE_CURVE('',#753,#753,#672,.T.);
#901=EDGE_CURVE('',#754,#754,#673,.T.);
#902=EDGE_CURVE('',#755,#755,#674,.T.);
#903=EDGE_CURVE('',#755,#754,#449,.T.);
#904=EDGE_CURVE('',#755,#756,#450,.T.);
#905=EDGE_CURVE('',#756,#756,#675,.T.);
#906=EDGE_CURVE('',#753,#757,#451,.T.);
#907=EDGE_CURVE('',#757,#757,#676,.T.);
#908=EDGE_CURVE('',#758,#758,#677,.T.);
#909=EDGE_CURVE('',#757,#758,#452,.T.);
#910=EDGE_CURVE('',#759,#759,#678,.T.);
#911=EDGE_CURVE('',#760,#760,#679,.T.);
#912=EDGE_CURVE('',#759,#761,#453,.T.);
#913=EDGE_CURVE('',#761,#761,#680,.T.);
#914=EDGE_CURVE('',#762,#762,#681,.T.);
#915=EDGE_CURVE('',#763,#763,#682,.T.);
#916=EDGE_CURVE('',#763,#762,#454,.T.);
#917=EDGE_CURVE('',#764,#764,#683,.T.);
#918=EDGE_CURVE('',#765,#765,#684,.T.);
#919=EDGE_CURVE('',#765,#764,#455,.T.);
#920=EDGE_CURVE('',#765,#766,#456,.T.);
#921=EDGE_CURVE('',#766,#766,#685,.T.);
#922=EDGE_CURVE('',#767,#767,#686,.T.);
#923=EDGE_CURVE('',#761,#767,#457,.T.);
#924=EDGE_CURVE('',#760,#768,#687,.T.);
#925=EDGE_CURVE('',#769,#770,#688,.T.);
#926=EDGE_CURVE('',#771,#772,#689,.T.);
#927=EDGE_CURVE('',#773,#774,#690,.T.);
#928=EDGE_CURVE('',#775,#775,#691,.T.);
#929=EDGE_CURVE('',#775,#776,#458,.T.);
#930=EDGE_CURVE('',#776,#776,#692,.T.);
#931=EDGE_CURVE('',#777,#778,#459,.T.);
#932=EDGE_CURVE('',#779,#777,#460,.T.);
#933=EDGE_CURVE('',#780,#779,#461,.T.);
#934=EDGE_CURVE('',#781,#780,#462,.T.);
#935=EDGE_CURVE('',#782,#781,#463,.T.);
#936=EDGE_CURVE('',#783,#782,#464,.T.);
#937=EDGE_CURVE('',#784,#783,#465,.T.);
#938=EDGE_CURVE('',#785,#784,#466,.T.);
#939=EDGE_CURVE('',#786,#785,#467,.T.);
#940=EDGE_CURVE('',#787,#786,#468,.T.);
#941=EDGE_CURVE('',#778,#787,#469,.T.);
#942=EDGE_CURVE('',#788,#788,#693,.T.);
#943=EDGE_CURVE('',#789,#789,#694,.T.);
#944=EDGE_CURVE('',#775,#790,#470,.T.);
#945=EDGE_CURVE('',#790,#790,#695,.T.);
#946=EDGE_CURVE('',#791,#791,#696,.T.);
#947=EDGE_CURVE('',#791,#788,#471,.T.);
#948=EDGE_CURVE('',#791,#792,#472,.T.);
#949=EDGE_CURVE('',#792,#792,#697,.T.);
#950=EDGE_CURVE('',#793,#794,#473,.T.);
#951=EDGE_CURVE('',#794,#777,#474,.T.);
#952=EDGE_CURVE('',#778,#793,#475,.T.);
#953=EDGE_CURVE('',#787,#795,#476,.T.);
#954=EDGE_CURVE('',#795,#793,#477,.T.);
#955=EDGE_CURVE('',#786,#796,#478,.T.);
#956=EDGE_CURVE('',#796,#795,#479,.T.);
#957=EDGE_CURVE('',#785,#797,#480,.F.);
#958=EDGE_CURVE('',#797,#796,#481,.T.);
#959=EDGE_CURVE('',#793,#798,#482,.T.);
#960=EDGE_CURVE('',#798,#799,#483,.T.);
#961=EDGE_CURVE('',#799,#794,#484,.T.);
#962=EDGE_CURVE('',#800,#795,#485,.T.);
#963=EDGE_CURVE('',#800,#798,#486,.T.);
#964=EDGE_CURVE('',#796,#801,#487,.T.);
#965=EDGE_CURVE('',#801,#800,#488,.T.);
#966=EDGE_CURVE('',#802,#797,#489,.T.);
#967=EDGE_CURVE('',#802,#801,#490,.F.);
#968=EDGE_CURVE('',#803,#802,#491,.T.);
#969=EDGE_CURVE('',#804,#803,#492,.T.);
#970=EDGE_CURVE('',#804,#805,#493,.T.);
#971=EDGE_CURVE('',#806,#805,#494,.T.);
#972=EDGE_CURVE('',#807,#806,#495,.T.);
#973=EDGE_CURVE('',#808,#807,#496,.T.);
#974=EDGE_CURVE('',#799,#808,#497,.F.);
#975=EDGE_CURVE('',#809,#809,#698,.T.);
#976=EDGE_CURVE('',#810,#797,#498,.T.);
#977=EDGE_CURVE('',#784,#810,#499,.T.);
#978=EDGE_CURVE('',#782,#811,#500,.T.);
#979=EDGE_CURVE('',#811,#812,#501,.T.);
#980=EDGE_CURVE('',#812,#783,#502,.T.);
#981=EDGE_CURVE('',#781,#813,#503,.T.);
#982=EDGE_CURVE('',#813,#811,#504,.T.);
#983=EDGE_CURVE('',#780,#814,#505,.T.);
#984=EDGE_CURVE('',#814,#813,#506,.T.);
#985=EDGE_CURVE('',#779,#815,#507,.T.);
#986=EDGE_CURVE('',#815,#814,#508,.T.);
#987=EDGE_CURVE('',#794,#815,#509,.T.);
#988=EDGE_CURVE('',#812,#810,#510,.T.);
#989=EDGE_CURVE('',#803,#810,#511,.T.);
#990=EDGE_CURVE('',#812,#804,#512,.T.);
#991=EDGE_CURVE('',#805,#811,#513,.T.);
#992=EDGE_CURVE('',#813,#806,#514,.T.);
#993=EDGE_CURVE('',#807,#814,#515,.T.);
#994=EDGE_CURVE('',#815,#808,#516,.T.);
#995=EDGE_CURVE('',#816,#816,#699,.T.);
#996=EDGE_CURVE('',#816,#789,#517,.T.);
#997=EDGE_CURVE('',#816,#809,#518,.T.);
#998=ORIENTED_EDGE('',*,*,#817,.T.);
#999=ORIENTED_EDGE('',*,*,#818,.T.);
#1000=ORIENTED_EDGE('',*,*,#819,.T.);
#1001=ORIENTED_EDGE('',*,*,#818,.F.);
#1002=ORIENTED_EDGE('',*,*,#820,.T.);
#1003=ORIENTED_EDGE('',*,*,#821,.T.);
#1004=ORIENTED_EDGE('',*,*,#822,.T.);
#1005=ORIENTED_EDGE('',*,*,#823,.T.);
#1006=ORIENTED_EDGE('',*,*,#824,.T.);
#1007=ORIENTED_EDGE('',*,*,#825,.F.);
#1008=ORIENTED_EDGE('',*,*,#826,.T.);
#1009=ORIENTED_EDGE('',*,*,#827,.F.);
#1010=ORIENTED_EDGE('',*,*,#819,.F.);
#1011=ORIENTED_EDGE('',*,*,#817,.F.);
#1012=ORIENTED_EDGE('',*,*,#828,.T.);
#1013=ORIENTED_EDGE('',*,*,#829,.T.);
#1014=ORIENTED_EDGE('',*,*,#828,.F.);
#1015=ORIENTED_EDGE('',*,*,#830,.T.);
#1016=ORIENTED_EDGE('',*,*,#831,.T.);
#1017=ORIENTED_EDGE('',*,*,#825,.T.);
#1018=ORIENTED_EDGE('',*,*,#831,.F.);
#1019=ORIENTED_EDGE('',*,*,#830,.F.);
#1020=ORIENTED_EDGE('',*,*,#832,.T.);
#1021=ORIENTED_EDGE('',*,*,#833,.T.);
#1022=ORIENTED_EDGE('',*,*,#832,.F.);
#1023=ORIENTED_EDGE('',*,*,#834,.T.);
#1024=ORIENTED_EDGE('',*,*,#835,.T.);
#1025=ORIENTED_EDGE('',*,*,#827,.T.);
#1026=ORIENTED_EDGE('',*,*,#835,.F.);
#1027=ORIENTED_EDGE('',*,*,#834,.F.);
#1028=ORIENTED_EDGE('',*,*,#836,.T.);
#1029=ORIENTED_EDGE('',*,*,#837,.T.);
#1030=ORIENTED_EDGE('',*,*,#836,.F.);
#1031=ORIENTED_EDGE('',*,*,#837,.F.);
#1032=ORIENTED_EDGE('',*,*,#833,.F.);
#1033=ORIENTED_EDGE('',*,*,#829,.F.);
#1034=ORIENTED_EDGE('',*,*,#838,.T.);
#1035=ORIENTED_EDGE('',*,*,#839,.T.);
#1036=ORIENTED_EDGE('',*,*,#826,.F.);
#1037=ORIENTED_EDGE('',*,*,#839,.F.);
#1038=ORIENTED_EDGE('',*,*,#840,.F.);
#1039=ORIENTED_EDGE('',*,*,#841,.T.);
#1040=ORIENTED_EDGE('',*,*,#824,.F.);
#1041=ORIENTED_EDGE('',*,*,#842,.F.);
#1042=ORIENTED_EDGE('',*,*,#843,.T.);
#1043=ORIENTED_EDGE('',*,*,#842,.T.);
#1044=ORIENTED_EDGE('',*,*,#823,.F.);
#1045=ORIENTED_EDGE('',*,*,#844,.F.);
#1046=ORIENTED_EDGE('',*,*,#845,.T.);
#1047=ORIENTED_EDGE('',*,*,#844,.T.);
#1048=ORIENTED_EDGE('',*,*,#822,.F.);
#1049=ORIENTED_EDGE('',*,*,#846,.F.);
#1050=ORIENTED_EDGE('',*,*,#847,.T.);
#1051=ORIENTED_EDGE('',*,*,#846,.T.);
#1052=ORIENTED_EDGE('',*,*,#821,.F.);
#1053=ORIENTED_EDGE('',*,*,#848,.F.);
#1054=ORIENTED_EDGE('',*,*,#849,.T.);
#1055=ORIENTED_EDGE('',*,*,#848,.T.);
#1056=ORIENTED_EDGE('',*,*,#820,.F.);
#1057=ORIENTED_EDGE('',*,*,#841,.F.);
#1058=ORIENTED_EDGE('',*,*,#849,.F.);
#1059=ORIENTED_EDGE('',*,*,#840,.T.);
#1060=ORIENTED_EDGE('',*,*,#843,.F.);
#1061=ORIENTED_EDGE('',*,*,#845,.F.);
#1062=ORIENTED_EDGE('',*,*,#847,.F.);
#1063=ORIENTED_EDGE('',*,*,#838,.F.);
#1064=ORIENTED_EDGE('',*,*,#850,.T.);
#1065=ORIENTED_EDGE('',*,*,#851,.T.);
#1066=ORIENTED_EDGE('',*,*,#852,.F.);
#1067=ORIENTED_EDGE('',*,*,#853,.T.);
#1068=ORIENTED_EDGE('',*,*,#851,.F.);
#1069=ORIENTED_EDGE('',*,*,#853,.F.);
#1070=ORIENTED_EDGE('',*,*,#852,.T.);
#1071=ORIENTED_EDGE('',*,*,#854,.T.);
#1072=ORIENTED_EDGE('',*,*,#855,.T.);
#1073=ORIENTED_EDGE('',*,*,#854,.F.);
#1074=ORIENTED_EDGE('',*,*,#850,.F.);
#1075=ORIENTED_EDGE('',*,*,#856,.T.);
#1076=ORIENTED_EDGE('',*,*,#857,.F.);
#1077=ORIENTED_EDGE('',*,*,#856,.F.);
#1078=ORIENTED_EDGE('',*,*,#858,.F.);
#1079=ORIENTED_EDGE('',*,*,#855,.F.);
#1080=ORIENTED_EDGE('',*,*,#857,.T.);
#1081=ORIENTED_EDGE('',*,*,#859,.T.);
#1082=ORIENTED_EDGE('',*,*,#858,.T.);
#1083=ORIENTED_EDGE('',*,*,#859,.F.);
#1084=ORIENTED_EDGE('',*,*,#860,.T.);
#1085=ORIENTED_EDGE('',*,*,#861,.T.);
#1086=ORIENTED_EDGE('',*,*,#860,.F.);
#1087=ORIENTED_EDGE('',*,*,#862,.T.);
#1088=ORIENTED_EDGE('',*,*,#863,.T.);
#1089=ORIENTED_EDGE('',*,*,#862,.F.);
#1090=ORIENTED_EDGE('',*,*,#864,.T.);
#1091=ORIENTED_EDGE('',*,*,#865,.T.);
#1092=ORIENTED_EDGE('',*,*,#866,.T.);
#1093=ORIENTED_EDGE('',*,*,#864,.F.);
#1094=ORIENTED_EDGE('',*,*,#866,.F.);
#1095=ORIENTED_EDGE('',*,*,#867,.F.);
#1096=ORIENTED_EDGE('',*,*,#865,.F.);
#1097=ORIENTED_EDGE('',*,*,#868,.F.);
#1098=ORIENTED_EDGE('',*,*,#869,.T.);
#1099=ORIENTED_EDGE('',*,*,#867,.T.);
#1100=ORIENTED_EDGE('',*,*,#869,.F.);
#1101=ORIENTED_EDGE('',*,*,#868,.T.);
#1102=ORIENTED_EDGE('',*,*,#870,.T.);
#1103=ORIENTED_EDGE('',*,*,#871,.T.);
#1104=ORIENTED_EDGE('',*,*,#870,.F.);
#1105=ORIENTED_EDGE('',*,*,#871,.F.);
#1106=ORIENTED_EDGE('',*,*,#872,.F.);
#1107=ORIENTED_EDGE('',*,*,#863,.F.);
#1108=ORIENTED_EDGE('',*,*,#873,.T.);
#1109=ORIENTED_EDGE('',*,*,#872,.T.);
#1110=ORIENTED_EDGE('',*,*,#873,.F.);
#1111=ORIENTED_EDGE('',*,*,#861,.F.);
#1112=ORIENTED_EDGE('',*,*,#874,.T.);
#1113=ORIENTED_EDGE('',*,*,#874,.F.);
#1114=ORIENTED_EDGE('',*,*,#875,.T.);
#1115=ORIENTED_EDGE('',*,*,#876,.T.);
#1116=ORIENTED_EDGE('',*,*,#877,.F.);
#1117=ORIENTED_EDGE('',*,*,#878,.T.);
#1118=ORIENTED_EDGE('',*,*,#876,.F.);
#1119=ORIENTED_EDGE('',*,*,#878,.F.);
#1120=ORIENTED_EDGE('',*,*,#877,.T.);
#1121=ORIENTED_EDGE('',*,*,#879,.T.);
#1122=ORIENTED_EDGE('',*,*,#880,.T.);
#1123=ORIENTED_EDGE('',*,*,#879,.F.);
#1124=ORIENTED_EDGE('',*,*,#875,.F.);
#1125=ORIENTED_EDGE('',*,*,#881,.T.);
#1126=ORIENTED_EDGE('',*,*,#882,.F.);
#1127=ORIENTED_EDGE('',*,*,#881,.F.);
#1128=ORIENTED_EDGE('',*,*,#883,.F.);
#1129=ORIENTED_EDGE('',*,*,#880,.F.);
#1130=ORIENTED_EDGE('',*,*,#882,.T.);
#1131=ORIENTED_EDGE('',*,*,#884,.T.);
#1132=ORIENTED_EDGE('',*,*,#883,.T.);
#1133=ORIENTED_EDGE('',*,*,#884,.F.);
#1134=ORIENTED_EDGE('',*,*,#885,.T.);
#1135=ORIENTED_EDGE('',*,*,#886,.T.);
#1136=ORIENTED_EDGE('',*,*,#885,.F.);
#1137=ORIENTED_EDGE('',*,*,#887,.T.);
#1138=ORIENTED_EDGE('',*,*,#888,.T.);
#1139=ORIENTED_EDGE('',*,*,#887,.F.);
#1140=ORIENTED_EDGE('',*,*,#889,.T.);
#1141=ORIENTED_EDGE('',*,*,#890,.T.);
#1142=ORIENTED_EDGE('',*,*,#891,.T.);
#1143=ORIENTED_EDGE('',*,*,#889,.F.);
#1144=ORIENTED_EDGE('',*,*,#891,.F.);
#1145=ORIENTED_EDGE('',*,*,#892,.F.);
#1146=ORIENTED_EDGE('',*,*,#890,.F.);
#1147=ORIENTED_EDGE('',*,*,#893,.F.);
#1148=ORIENTED_EDGE('',*,*,#894,.T.);
#1149=ORIENTED_EDGE('',*,*,#892,.T.);
#1150=ORIENTED_EDGE('',*,*,#894,.F.);
#1151=ORIENTED_EDGE('',*,*,#893,.T.);
#1152=ORIENTED_EDGE('',*,*,#895,.T.);
#1153=ORIENTED_EDGE('',*,*,#896,.T.);
#1154=ORIENTED_EDGE('',*,*,#895,.F.);
#1155=ORIENTED_EDGE('',*,*,#896,.F.);
#1156=ORIENTED_EDGE('',*,*,#897,.F.);
#1157=ORIENTED_EDGE('',*,*,#888,.F.);
#1158=ORIENTED_EDGE('',*,*,#898,.T.);
#1159=ORIENTED_EDGE('',*,*,#897,.T.);
#1160=ORIENTED_EDGE('',*,*,#898,.F.);
#1161=ORIENTED_EDGE('',*,*,#886,.F.);
#1162=ORIENTED_EDGE('',*,*,#899,.T.);
#1163=ORIENTED_EDGE('',*,*,#899,.F.);
#1164=ORIENTED_EDGE('',*,*,#900,.T.);
#1165=ORIENTED_EDGE('',*,*,#901,.T.);
#1166=ORIENTED_EDGE('',*,*,#902,.F.);
#1167=ORIENTED_EDGE('',*,*,#903,.T.);
#1168=ORIENTED_EDGE('',*,*,#901,.F.);
#1169=ORIENTED_EDGE('',*,*,#903,.F.);
#1170=ORIENTED_EDGE('',*,*,#902,.T.);
#1171=ORIENTED_EDGE('',*,*,#904,.T.);
#1172=ORIENTED_EDGE('',*,*,#905,.T.);
#1173=ORIENTED_EDGE('',*,*,#904,.F.);
#1174=ORIENTED_EDGE('',*,*,#900,.F.);
#1175=ORIENTED_EDGE('',*,*,#906,.T.);
#1176=ORIENTED_EDGE('',*,*,#907,.F.);
#1177=ORIENTED_EDGE('',*,*,#906,.F.);
#1178=ORIENTED_EDGE('',*,*,#908,.F.);
#1179=ORIENTED_EDGE('',*,*,#905,.F.);
#1180=ORIENTED_EDGE('',*,*,#907,.T.);
#1181=ORIENTED_EDGE('',*,*,#909,.T.);
#1182=ORIENTED_EDGE('',*,*,#908,.T.);
#1183=ORIENTED_EDGE('',*,*,#909,.F.);
#1184=ORIENTED_EDGE('',*,*,#910,.T.);
#1185=ORIENTED_EDGE('',*,*,#911,.T.);
#1186=ORIENTED_EDGE('',*,*,#910,.F.);
#1187=ORIENTED_EDGE('',*,*,#912,.T.);
#1188=ORIENTED_EDGE('',*,*,#913,.T.);
#1189=ORIENTED_EDGE('',*,*,#912,.F.);
#1190=ORIENTED_EDGE('',*,*,#914,.T.);
#1191=ORIENTED_EDGE('',*,*,#915,.T.);
#1192=ORIENTED_EDGE('',*,*,#916,.T.);
#1193=ORIENTED_EDGE('',*,*,#914,.F.);
#1194=ORIENTED_EDGE('',*,*,#916,.F.);
#1195=ORIENTED_EDGE('',*,*,#917,.F.);
#1196=ORIENTED_EDGE('',*,*,#915,.F.);
#1197=ORIENTED_EDGE('',*,*,#918,.F.);
#1198=ORIENTED_EDGE('',*,*,#919,.T.);
#1199=ORIENTED_EDGE('',*,*,#917,.T.);
#1200=ORIENTED_EDGE('',*,*,#919,.F.);
#1201=ORIENTED_EDGE('',*,*,#918,.T.);
#1202=ORIENTED_EDGE('',*,*,#920,.T.);
#1203=ORIENTED_EDGE('',*,*,#921,.T.);
#1204=ORIENTED_EDGE('',*,*,#920,.F.);
#1205=ORIENTED_EDGE('',*,*,#921,.F.);
#1206=ORIENTED_EDGE('',*,*,#922,.F.);
#1207=ORIENTED_EDGE('',*,*,#913,.F.);
#1208=ORIENTED_EDGE('',*,*,#923,.T.);
#1209=ORIENTED_EDGE('',*,*,#922,.T.);
#1210=ORIENTED_EDGE('',*,*,#923,.F.);
#1211=ORIENTED_EDGE('',*,*,#911,.F.);
#1212=ORIENTED_EDGE('',*,*,#924,.T.);
#1213=ORIENTED_EDGE('',*,*,#924,.F.);
#1214=ORIENTED_EDGE('',*,*,#925,.T.);
#1215=ORIENTED_EDGE('',*,*,#925,.F.);
#1216=ORIENTED_EDGE('',*,*,#926,.T.);
#1217=ORIENTED_EDGE('',*,*,#926,.F.);
#1218=ORIENTED_EDGE('',*,*,#927,.T.);
#1219=ORIENTED_EDGE('',*,*,#927,.F.);
#1220=ORIENTED_EDGE('',*,*,#928,.T.);
#1221=ORIENTED_EDGE('',*,*,#929,.T.);
#1222=ORIENTED_EDGE('',*,*,#930,.T.);
#1223=ORIENTED_EDGE('',*,*,#929,.F.);
#1224=ORIENTED_EDGE('',*,*,#931,.F.);
#1225=ORIENTED_EDGE('',*,*,#932,.F.);
#1226=ORIENTED_EDGE('',*,*,#933,.F.);
#1227=ORIENTED_EDGE('',*,*,#934,.F.);
#1228=ORIENTED_EDGE('',*,*,#935,.F.);
#1229=ORIENTED_EDGE('',*,*,#936,.F.);
#1230=ORIENTED_EDGE('',*,*,#937,.F.);
#1231=ORIENTED_EDGE('',*,*,#938,.F.);
#1232=ORIENTED_EDGE('',*,*,#939,.F.);
#1233=ORIENTED_EDGE('',*,*,#940,.F.);
#1234=ORIENTED_EDGE('',*,*,#941,.F.);
#1235=ORIENTED_EDGE('',*,*,#942,.F.);
#1236=ORIENTED_EDGE('',*,*,#943,.F.);
#1237=ORIENTED_EDGE('',*,*,#930,.F.);
#1238=ORIENTED_EDGE('',*,*,#928,.F.);
#1239=ORIENTED_EDGE('',*,*,#944,.T.);
#1240=ORIENTED_EDGE('',*,*,#945,.F.);
#1241=ORIENTED_EDGE('',*,*,#944,.F.);
#1242=ORIENTED_EDGE('',*,*,#946,.T.);
#1243=ORIENTED_EDGE('',*,*,#947,.T.);
#1244=ORIENTED_EDGE('',*,*,#942,.T.);
#1245=ORIENTED_EDGE('',*,*,#947,.F.);
#1246=ORIENTED_EDGE('',*,*,#946,.F.);
#1247=ORIENTED_EDGE('',*,*,#948,.T.);
#1248=ORIENTED_EDGE('',*,*,#949,.F.);
#1249=ORIENTED_EDGE('',*,*,#948,.F.);
#1250=ORIENTED_EDGE('',*,*,#950,.T.);
#1251=ORIENTED_EDGE('',*,*,#951,.T.);
#1252=ORIENTED_EDGE('',*,*,#931,.T.);
#1253=ORIENTED_EDGE('',*,*,#952,.T.);
#1254=ORIENTED_EDGE('',*,*,#941,.T.);
#1255=ORIENTED_EDGE('',*,*,#953,.T.);
#1256=ORIENTED_EDGE('',*,*,#954,.T.);
#1257=ORIENTED_EDGE('',*,*,#952,.F.);
#1258=ORIENTED_EDGE('',*,*,#940,.T.);
#1259=ORIENTED_EDGE('',*,*,#955,.T.);
#1260=ORIENTED_EDGE('',*,*,#956,.T.);
#1261=ORIENTED_EDGE('',*,*,#953,.F.);
#1262=ORIENTED_EDGE('',*,*,#939,.T.);
#1263=ORIENTED_EDGE('',*,*,#957,.T.);
#1264=ORIENTED_EDGE('',*,*,#958,.T.);
#1265=ORIENTED_EDGE('',*,*,#955,.F.);
#1266=ORIENTED_EDGE('',*,*,#950,.F.);
#1267=ORIENTED_EDGE('',*,*,#959,.T.);
#1268=ORIENTED_EDGE('',*,*,#960,.T.);
#1269=ORIENTED_EDGE('',*,*,#961,.T.);
#1270=ORIENTED_EDGE('',*,*,#954,.F.);
#1271=ORIENTED_EDGE('',*,*,#962,.F.);
#1272=ORIENTED_EDGE('',*,*,#963,.T.);
#1273=ORIENTED_EDGE('',*,*,#959,.F.);
#1274=ORIENTED_EDGE('',*,*,#956,.F.);
#1275=ORIENTED_EDGE('',*,*,#964,.T.);
#1276=ORIENTED_EDGE('',*,*,#965,.T.);
#1277=ORIENTED_EDGE('',*,*,#962,.T.);
#1278=ORIENTED_EDGE('',*,*,#958,.F.);
#1279=ORIENTED_EDGE('',*,*,#966,.F.);
#1280=ORIENTED_EDGE('',*,*,#967,.T.);
#1281=ORIENTED_EDGE('',*,*,#964,.F.);
#1282=ORIENTED_EDGE('',*,*,#965,.F.);
#1283=ORIENTED_EDGE('',*,*,#967,.F.);
#1284=ORIENTED_EDGE('',*,*,#968,.F.);
#1285=ORIENTED_EDGE('',*,*,#969,.F.);
#1286=ORIENTED_EDGE('',*,*,#970,.T.);
#1287=ORIENTED_EDGE('',*,*,#971,.F.);
#1288=ORIENTED_EDGE('',*,*,#972,.F.);
#1289=ORIENTED_EDGE('',*,*,#973,.F.);
#1290=ORIENTED_EDGE('',*,*,#974,.F.);
#1291=ORIENTED_EDGE('',*,*,#960,.F.);
#1292=ORIENTED_EDGE('',*,*,#963,.F.);
#1293=ORIENTED_EDGE('',*,*,#945,.T.);
#1294=ORIENTED_EDGE('',*,*,#949,.T.);
#1295=ORIENTED_EDGE('',*,*,#975,.T.);
#1296=ORIENTED_EDGE('',*,*,#976,.T.);
#1297=ORIENTED_EDGE('',*,*,#957,.F.);
#1298=ORIENTED_EDGE('',*,*,#938,.T.);
#1299=ORIENTED_EDGE('',*,*,#977,.T.);
#1300=ORIENTED_EDGE('',*,*,#936,.T.);
#1301=ORIENTED_EDGE('',*,*,#978,.T.);
#1302=ORIENTED_EDGE('',*,*,#979,.T.);
#1303=ORIENTED_EDGE('',*,*,#980,.T.);
#1304=ORIENTED_EDGE('',*,*,#935,.T.);
#1305=ORIENTED_EDGE('',*,*,#981,.T.);
#1306=ORIENTED_EDGE('',*,*,#982,.T.);
#1307=ORIENTED_EDGE('',*,*,#978,.F.);
#1308=ORIENTED_EDGE('',*,*,#934,.T.);
#1309=ORIENTED_EDGE('',*,*,#983,.T.);
#1310=ORIENTED_EDGE('',*,*,#984,.T.);
#1311=ORIENTED_EDGE('',*,*,#981,.F.);
#1312=ORIENTED_EDGE('',*,*,#933,.T.);
#1313=ORIENTED_EDGE('',*,*,#985,.T.);
#1314=ORIENTED_EDGE('',*,*,#986,.T.);
#1315=ORIENTED_EDGE('',*,*,#983,.F.);
#1316=ORIENTED_EDGE('',*,*,#951,.F.);
#1317=ORIENTED_EDGE('',*,*,#987,.T.);
#1318=ORIENTED_EDGE('',*,*,#985,.F.);
#1319=ORIENTED_EDGE('',*,*,#932,.T.);
#1320=ORIENTED_EDGE('',*,*,#937,.T.);
#1321=ORIENTED_EDGE('',*,*,#980,.F.);
#1322=ORIENTED_EDGE('',*,*,#988,.T.);
#1323=ORIENTED_EDGE('',*,*,#977,.F.);
#1324=ORIENTED_EDGE('',*,*,#976,.F.);
#1325=ORIENTED_EDGE('',*,*,#989,.F.);
#1326=ORIENTED_EDGE('',*,*,#968,.T.);
#1327=ORIENTED_EDGE('',*,*,#966,.T.);
#1328=ORIENTED_EDGE('',*,*,#988,.F.);
#1329=ORIENTED_EDGE('',*,*,#990,.T.);
#1330=ORIENTED_EDGE('',*,*,#969,.T.);
#1331=ORIENTED_EDGE('',*,*,#989,.T.);
#1332=ORIENTED_EDGE('',*,*,#979,.F.);
#1333=ORIENTED_EDGE('',*,*,#991,.F.);
#1334=ORIENTED_EDGE('',*,*,#970,.F.);
#1335=ORIENTED_EDGE('',*,*,#990,.F.);
#1336=ORIENTED_EDGE('',*,*,#982,.F.);
#1337=ORIENTED_EDGE('',*,*,#992,.T.);
#1338=ORIENTED_EDGE('',*,*,#971,.T.);
#1339=ORIENTED_EDGE('',*,*,#991,.T.);
#1340=ORIENTED_EDGE('',*,*,#984,.F.);
#1341=ORIENTED_EDGE('',*,*,#993,.F.);
#1342=ORIENTED_EDGE('',*,*,#972,.T.);
#1343=ORIENTED_EDGE('',*,*,#992,.F.);
#1344=ORIENTED_EDGE('',*,*,#986,.F.);
#1345=ORIENTED_EDGE('',*,*,#994,.T.);
#1346=ORIENTED_EDGE('',*,*,#973,.T.);
#1347=ORIENTED_EDGE('',*,*,#993,.T.);
#1348=ORIENTED_EDGE('',*,*,#987,.F.);
#1349=ORIENTED_EDGE('',*,*,#961,.F.);
#1350=ORIENTED_EDGE('',*,*,#974,.T.);
#1351=ORIENTED_EDGE('',*,*,#994,.F.);
#1352=ORIENTED_EDGE('',*,*,#995,.T.);
#1353=ORIENTED_EDGE('',*,*,#996,.T.);
#1354=ORIENTED_EDGE('',*,*,#943,.T.);
#1355=ORIENTED_EDGE('',*,*,#996,.F.);
#1356=ORIENTED_EDGE('',*,*,#995,.F.);
#1357=ORIENTED_EDGE('',*,*,#997,.T.);
#1358=ORIENTED_EDGE('',*,*,#975,.F.);
#1359=ORIENTED_EDGE('',*,*,#997,.F.);
#1360=CONICAL_SURFACE('',#1578,2.25,0.785398163397449);
#1361=CONICAL_SURFACE('',#1587,2.25,0.785398163397449);
#1362=CONICAL_SURFACE('',#1591,2.25,0.785398163397449);
#1363=CONICAL_SURFACE('',#1612,1.1,0.785398163397448);
#1364=CONICAL_SURFACE('',#1618,1.9,0.785398163397448);
#1365=CONICAL_SURFACE('',#1632,1.9,0.785398163397448);
#1366=CONICAL_SURFACE('',#1636,1.1,0.785398163397448);
#1367=CONICAL_SURFACE('',#1645,1.1,0.785398163397448);
#1368=CONICAL_SURFACE('',#1651,1.9,0.785398163397448);
#1369=CONICAL_SURFACE('',#1665,1.9,0.785398163397448);
#1370=CONICAL_SURFACE('',#1669,1.1,0.785398163397448);
#1371=CONICAL_SURFACE('',#1678,1.1,0.785398163397448);
#1372=CONICAL_SURFACE('',#1684,1.9,0.785398163397448);
#1373=CONICAL_SURFACE('',#1698,1.9,0.785398163397448);
#1374=CONICAL_SURFACE('',#1702,1.1,0.785398163397448);
#1375=CONICAL_SURFACE('',#1715,2.15,0.785398163397448);
#1376=CONICAL_SURFACE('',#1723,2.15,0.785398163397448);
#1377=CONICAL_SURFACE('',#1751,2.15,0.785398163397448);
#1378=ADVANCED_FACE('',(#187),#1360,.F.);
#1379=ADVANCED_FACE('',(#188,#109,#110,#111,#112),#135,.T.);
#1380=ADVANCED_FACE('',(#189),#87,.F.);
#1381=ADVANCED_FACE('',(#190),#1361,.F.);
#1382=ADVANCED_FACE('',(#191),#88,.F.);
#1383=ADVANCED_FACE('',(#192),#1362,.F.);
#1384=ADVANCED_FACE('',(#193),#89,.F.);
#1385=ADVANCED_FACE('',(#194),#136,.T.);
#1386=ADVANCED_FACE('',(#195),#137,.T.);
#1387=ADVANCED_FACE('',(#196),#138,.T.);
#1388=ADVANCED_FACE('',(#197),#90,.F.);
#1389=ADVANCED_FACE('',(#198),#139,.T.);
#1390=ADVANCED_FACE('',(#199),#140,.T.);
#1391=ADVANCED_FACE('',(#200),#141,.T.);
#1392=ADVANCED_FACE('',(#201),#142,.T.);
#1393=ADVANCED_FACE('',(#202),#143,.T.);
#1394=ADVANCED_FACE('',(#203,#113),#144,.F.);
#1395=ADVANCED_FACE('',(#204,#114),#145,.F.);
#1396=ADVANCED_FACE('',(#205),#91,.F.);
#1397=ADVANCED_FACE('',(#206),#1363,.F.);
#1398=ADVANCED_FACE('',(#207),#92,.T.);
#1399=ADVANCED_FACE('',(#208,#115),#146,.T.);
#1400=ADVANCED_FACE('',(#209),#1364,.T.);
#1401=ADVANCED_FACE('',(#210,#116),#147,.F.);
#1402=ADVANCED_FACE('',(#211),#93,.T.);
#1403=ADVANCED_FACE('',(#212),#148,.T.);
#1404=ADVANCED_FACE('',(#213),#94,.T.);
#1405=ADVANCED_FACE('',(#214,#117),#149,.T.);
#1406=ADVANCED_FACE('',(#215),#95,.T.);
#1407=ADVANCED_FACE('',(#216),#1365,.T.);
#1408=ADVANCED_FACE('',(#217,#118),#150,.F.);
#1409=ADVANCED_FACE('',(#218),#1366,.F.);
#1410=ADVANCED_FACE('',(#219),#43,.F.);
#1411=ADVANCED_FACE('',(#220,#119),#151,.F.);
#1412=ADVANCED_FACE('',(#221),#96,.F.);
#1413=ADVANCED_FACE('',(#222),#1367,.F.);
#1414=ADVANCED_FACE('',(#223),#97,.T.);
#1415=ADVANCED_FACE('',(#224,#120),#152,.T.);
#1416=ADVANCED_FACE('',(#225),#1368,.T.);
#1417=ADVANCED_FACE('',(#226,#121),#153,.F.);
#1418=ADVANCED_FACE('',(#227),#98,.T.);
#1419=ADVANCED_FACE('',(#228),#154,.T.);
#1420=ADVANCED_FACE('',(#229),#99,.T.);
#1421=ADVANCED_FACE('',(#230,#122),#155,.T.);
#1422=ADVANCED_FACE('',(#231),#100,.T.);
#1423=ADVANCED_FACE('',(#232),#1369,.T.);
#1424=ADVANCED_FACE('',(#233,#123),#156,.F.);
#1425=ADVANCED_FACE('',(#234),#1370,.F.);
#1426=ADVANCED_FACE('',(#235),#44,.F.);
#1427=ADVANCED_FACE('',(#236,#124),#157,.F.);
#1428=ADVANCED_FACE('',(#237),#101,.F.);
#1429=ADVANCED_FACE('',(#238),#1371,.F.);
#1430=ADVANCED_FACE('',(#239),#102,.T.);
#1431=ADVANCED_FACE('',(#240,#125),#158,.T.);
#1432=ADVANCED_FACE('',(#241),#1372,.T.);
#1433=ADVANCED_FACE('',(#242,#126),#159,.F.);
#1434=ADVANCED_FACE('',(#243),#103,.T.);
#1435=ADVANCED_FACE('',(#244),#160,.T.);
#1436=ADVANCED_FACE('',(#245),#104,.T.);
#1437=ADVANCED_FACE('',(#246,#127),#161,.T.);
#1438=ADVANCED_FACE('',(#247),#105,.T.);
#1439=ADVANCED_FACE('',(#248),#1373,.T.);
#1440=ADVANCED_FACE('',(#249,#128),#162,.F.);
#1441=ADVANCED_FACE('',(#250),#1374,.F.);
#1442=ADVANCED_FACE('',(#251),#45,.F.);
#1443=ADVANCED_FACE('',(#252),#46,.T.);
#1444=ADVANCED_FACE('',(#253),#47,.T.);
#1445=ADVANCED_FACE('',(#254),#48,.T.);
#1446=ADVANCED_FACE('',(#255),#1375,.F.);
#1447=ADVANCED_FACE('',(#256,#129,#130,#131),#163,.T.);
#1448=ADVANCED_FACE('',(#257),#106,.F.);
#1449=ADVANCED_FACE('',(#258),#1376,.F.);
#1450=ADVANCED_FACE('',(#259),#107,.F.);
#1451=ADVANCED_FACE('',(#260),#164,.T.);
#1452=ADVANCED_FACE('',(#261),#165,.T.);
#1453=ADVANCED_FACE('',(#262),#166,.T.);
#1454=ADVANCED_FACE('',(#263),#167,.T.);
#1455=ADVANCED_FACE('',(#264),#168,.T.);
#1456=ADVANCED_FACE('',(#265),#169,.T.);
#1457=ADVANCED_FACE('',(#266),#170,.T.);
#1458=ADVANCED_FACE('',(#267),#171,.T.);
#1459=ADVANCED_FACE('',(#268,#132,#133,#134),#172,.F.);
#1460=ADVANCED_FACE('',(#269),#173,.T.);
#1461=ADVANCED_FACE('',(#270),#174,.T.);
#1462=ADVANCED_FACE('',(#271),#175,.T.);
#1463=ADVANCED_FACE('',(#272),#176,.T.);
#1464=ADVANCED_FACE('',(#273),#177,.T.);
#1465=ADVANCED_FACE('',(#274),#178,.T.);
#1466=ADVANCED_FACE('',(#275),#179,.T.);
#1467=ADVANCED_FACE('',(#276),#180,.T.);
#1468=ADVANCED_FACE('',(#277),#181,.T.);
#1469=ADVANCED_FACE('',(#278),#182,.T.);
#1470=ADVANCED_FACE('',(#279),#183,.T.);
#1471=ADVANCED_FACE('',(#280),#184,.T.);
#1472=ADVANCED_FACE('',(#281),#185,.T.);
#1473=ADVANCED_FACE('',(#282),#186,.T.);
#1474=ADVANCED_FACE('',(#283),#1377,.F.);
#1475=ADVANCED_FACE('',(#284),#108,.F.);
#1476=CLOSED_SHELL('',(#1378,#1379,#1380,#1381,#1382,#1383,#1384,#1385,
#1386,#1387,#1388,#1389,#1390,#1391,#1392,#1393,#1394));
#1477=CLOSED_SHELL('',(#1395,#1396,#1397,#1398,#1399,#1400));
#1478=CLOSED_SHELL('',(#1401,#1402,#1403,#1404,#1405,#1406,#1407,#1408,
#1409,#1410));
#1479=CLOSED_SHELL('',(#1411,#1412,#1413,#1414,#1415,#1416));
#1480=CLOSED_SHELL('',(#1417,#1418,#1419,#1420,#1421,#1422,#1423,#1424,
#1425,#1426));
#1481=CLOSED_SHELL('',(#1427,#1428,#1429,#1430,#1431,#1432));
#1482=CLOSED_SHELL('',(#1433,#1434,#1435,#1436,#1437,#1438,#1439,#1440,
#1441,#1442));
#1483=CLOSED_SHELL('',(#1443));
#1484=CLOSED_SHELL('',(#1444));
#1485=CLOSED_SHELL('',(#1445));
#1486=CLOSED_SHELL('',(#1446,#1447,#1448,#1449,#1450,#1451,#1452,#1453,
#1454,#1455,#1456,#1457,#1458,#1459,#1460,#1461,#1462,#1463,#1464,#1465,
#1466,#1467,#1468,#1469,#1470,#1471,#1472,#1473,#1474,#1475));
#1487=DERIVED_UNIT_ELEMENT(#1503,1.);
#1488=DERIVED_UNIT_ELEMENT(#2678,-3.);
#1489=DERIVED_UNIT_ELEMENT(#1503,1.);
#1490=DERIVED_UNIT_ELEMENT(#2678,-3.);
#1491=DERIVED_UNIT_ELEMENT(#1503,1.);
#1492=DERIVED_UNIT_ELEMENT(#2678,-3.);
#1493=DERIVED_UNIT_ELEMENT(#1503,1.);
#1494=DERIVED_UNIT_ELEMENT(#2678,-3.);
#1495=DERIVED_UNIT_ELEMENT(#1503,1.);
#1496=DERIVED_UNIT_ELEMENT(#2678,-3.);
#1497=DERIVED_UNIT_ELEMENT(#1503,1.);
#1498=DERIVED_UNIT_ELEMENT(#2678,-3.);
#1499=DERIVED_UNIT_ELEMENT(#1503,1.);
#1500=DERIVED_UNIT_ELEMENT(#2678,-3.);
#1501=DERIVED_UNIT_ELEMENT(#1503,1.);
#1502=DERIVED_UNIT_ELEMENT(#2678,-3.);
#1503=(
MASS_UNIT()
NAMED_UNIT(*)
SI_UNIT(.KILO.,.GRAM.)
);
#1504=DERIVED_UNIT((#1487,#1488));
#1505=DERIVED_UNIT((#1489,#1490));
#1506=DERIVED_UNIT((#1491,#1492));
#1507=DERIVED_UNIT((#1493,#1494));
#1508=DERIVED_UNIT((#1495,#1496));
#1509=DERIVED_UNIT((#1497,#1498));
#1510=DERIVED_UNIT((#1499,#1500));
#1511=DERIVED_UNIT((#1501,#1502));
#1512=MEASURE_REPRESENTATION_ITEM('density measure',
POSITIVE_RATIO_MEASURE(7850.),#1504);
#1513=MEASURE_REPRESENTATION_ITEM('density measure',
POSITIVE_RATIO_MEASURE(7850.),#1505);
#1514=MEASURE_REPRESENTATION_ITEM('density measure',
POSITIVE_RATIO_MEASURE(7850.),#1506);
#1515=MEASURE_REPRESENTATION_ITEM('density measure',
POSITIVE_RATIO_MEASURE(7850.),#1507);
#1516=MEASURE_REPRESENTATION_ITEM('density measure',
POSITIVE_RATIO_MEASURE(7850.),#1508);
#1517=MEASURE_REPRESENTATION_ITEM('density measure',
POSITIVE_RATIO_MEASURE(7850.),#1509);
#1518=MEASURE_REPRESENTATION_ITEM('density measure',
POSITIVE_RATIO_MEASURE(7850.),#1510);
#1519=MEASURE_REPRESENTATION_ITEM('density measure',
POSITIVE_RATIO_MEASURE(7850.),#1511);
#1520=PROPERTY_DEFINITION_REPRESENTATION(#1560,#1536);
#1521=PROPERTY_DEFINITION_REPRESENTATION(#1561,#1537);
#1522=PROPERTY_DEFINITION_REPRESENTATION(#1562,#1538);
#1523=PROPERTY_DEFINITION_REPRESENTATION(#1563,#1539);
#1524=PROPERTY_DEFINITION_REPRESENTATION(#1564,#1540);
#1525=PROPERTY_DEFINITION_REPRESENTATION(#1565,#1541);
#1526=PROPERTY_DEFINITION_REPRESENTATION(#1566,#1542);
#1527=PROPERTY_DEFINITION_REPRESENTATION(#1567,#1543);
#1528=PROPERTY_DEFINITION_REPRESENTATION(#1568,#1544);
#1529=PROPERTY_DEFINITION_REPRESENTATION(#1569,#1545);
#1530=PROPERTY_DEFINITION_REPRESENTATION(#1570,#1546);
#1531=PROPERTY_DEFINITION_REPRESENTATION(#1571,#1547);
#1532=PROPERTY_DEFINITION_REPRESENTATION(#1572,#1548);
#1533=PROPERTY_DEFINITION_REPRESENTATION(#1573,#1549);
#1534=PROPERTY_DEFINITION_REPRESENTATION(#1574,#1550);
#1535=PROPERTY_DEFINITION_REPRESENTATION(#1575,#1551);
#1536=REPRESENTATION('material name',(#1552),#2668);
#1537=REPRESENTATION('density',(#1512),#2668);
#1538=REPRESENTATION('material name',(#1553),#2669);
#1539=REPRESENTATION('density',(#1513),#2669);
#1540=REPRESENTATION('material name',(#1554),#2670);
#1541=REPRESENTATION('density',(#1514),#2670);
#1542=REPRESENTATION('material name',(#1555),#2671);
#1543=REPRESENTATION('density',(#1515),#2671);
#1544=REPRESENTATION('material name',(#1556),#2672);
#1545=REPRESENTATION('density',(#1516),#2672);
#1546=REPRESENTATION('material name',(#1557),#2673);
#1547=REPRESENTATION('density',(#1517),#2673);
#1548=REPRESENTATION('material name',(#1558),#2674);
#1549=REPRESENTATION('density',(#1518),#2674);
#1550=REPRESENTATION('material name',(#1559),#2675);
#1551=REPRESENTATION('density',(#1519),#2675);
#1552=DESCRIPTIVE_REPRESENTATION_ITEM('Steel','Steel');
#1553=DESCRIPTIVE_REPRESENTATION_ITEM('Steel','Steel');
#1554=DESCRIPTIVE_REPRESENTATION_ITEM('Steel','Steel');
#1555=DESCRIPTIVE_REPRESENTATION_ITEM('Steel','Steel');
#1556=DESCRIPTIVE_REPRESENTATION_ITEM('Steel','Steel');
#1557=DESCRIPTIVE_REPRESENTATION_ITEM('Steel','Steel');
#1558=DESCRIPTIVE_REPRESENTATION_ITEM('Steel','Steel');
#1559=DESCRIPTIVE_REPRESENTATION_ITEM('Steel','Steel');
#1560=PROPERTY_DEFINITION('material property','material name',#2718);
#1561=PROPERTY_DEFINITION('material property','density of part',#2718);
#1562=PROPERTY_DEFINITION('material property','material name',#2719);
#1563=PROPERTY_DEFINITION('material property','density of part',#2719);
#1564=PROPERTY_DEFINITION('material property','material name',#2720);
#1565=PROPERTY_DEFINITION('material property','density of part',#2720);
#1566=PROPERTY_DEFINITION('material property','material name',#2721);
#1567=PROPERTY_DEFINITION('material property','density of part',#2721);
#1568=PROPERTY_DEFINITION('material property','material name',#2722);
#1569=PROPERTY_DEFINITION('material property','density of part',#2722);
#1570=PROPERTY_DEFINITION('material property','material name',#2723);
#1571=PROPERTY_DEFINITION('material property','density of part',#2723);
#1572=PROPERTY_DEFINITION('material property','material name',#2724);
#1573=PROPERTY_DEFINITION('material property','density of part',#2724);
#1574=PROPERTY_DEFINITION('material property','material name',#2725);
#1575=PROPERTY_DEFINITION('material property','density of part',#2725);
#1576=AXIS2_PLACEMENT_3D('',#2244,#1762,#1763);
#1577=AXIS2_PLACEMENT_3D('',#2245,#1764,#1765);
#1578=AXIS2_PLACEMENT_3D('',#2246,#1766,#1767);
#1579=AXIS2_PLACEMENT_3D('',#2248,#1768,#1769);
#1580=AXIS2_PLACEMENT_3D('',#2251,#1771,#1772);
#1581=AXIS2_PLACEMENT_3D('',#2252,#1773,#1774);
#1582=AXIS2_PLACEMENT_3D('',#2264,#1780,#1781);
#1583=AXIS2_PLACEMENT_3D('',#2266,#1782,#1783);
#1584=AXIS2_PLACEMENT_3D('',#2268,#1784,#1785);
#1585=AXIS2_PLACEMENT_3D('',#2269,#1786,#1787);
#1586=AXIS2_PLACEMENT_3D('',#2272,#1789,#1790);
#1587=AXIS2_PLACEMENT_3D('',#2273,#1791,#1792);
#1588=AXIS2_PLACEMENT_3D('',#2275,#1793,#1794);
#1589=AXIS2_PLACEMENT_3D('',#2277,#1796,#1797);
#1590=AXIS2_PLACEMENT_3D('',#2280,#1799,#1800);
#1591=AXIS2_PLACEMENT_3D('',#2281,#1801,#1802);
#1592=AXIS2_PLACEMENT_3D('',#2283,#1803,#1804);
#1593=AXIS2_PLACEMENT_3D('',#2285,#1806,#1807);
#1594=AXIS2_PLACEMENT_3D('',#2288,#1809,#1810);
#1595=AXIS2_PLACEMENT_3D('',#2289,#1811,#1812);
#1596=AXIS2_PLACEMENT_3D('',#2290,#1813,#1814);
#1597=AXIS2_PLACEMENT_3D('',#2291,#1815,#1816);
#1598=AXIS2_PLACEMENT_3D('',#2292,#1817,#1818);
#1599=AXIS2_PLACEMENT_3D('',#2294,#1819,#1820);
#1600=AXIS2_PLACEMENT_3D('',#2296,#1822,#1823);
#1601=AXIS2_PLACEMENT_3D('',#2302,#1827,#1828);
#1602=AXIS2_PLACEMENT_3D('',#2306,#1831,#1832);
#1603=AXIS2_PLACEMENT_3D('',#2310,#1835,#1836);
#1604=AXIS2_PLACEMENT_3D('',#2314,#1839,#1840);
#1605=AXIS2_PLACEMENT_3D('',#2316,#1842,#1843);
#1606=AXIS2_PLACEMENT_3D('',#2317,#1844,#1845);
#1607=AXIS2_PLACEMENT_3D('',#2318,#1846,#1847);
#1608=AXIS2_PLACEMENT_3D('',#2320,#1848,#1849);
#1609=AXIS2_PLACEMENT_3D('',#2322,#1850,#1851);
#1610=AXIS2_PLACEMENT_3D('',#2323,#1852,#1853);
#1611=AXIS2_PLACEMENT_3D('',#2325,#1854,#1855);
#1612=AXIS2_PLACEMENT_3D('',#2327,#1857,#1858);
#1613=AXIS2_PLACEMENT_3D('',#2330,#1860,#1861);
#1614=AXIS2_PLACEMENT_3D('',#2331,#1862,#1863);
#1615=AXIS2_PLACEMENT_3D('',#2334,#1865,#1866);
#1616=AXIS2_PLACEMENT_3D('',#2335,#1867,#1868);
#1617=AXIS2_PLACEMENT_3D('',#2337,#1869,#1870);
#1618=AXIS2_PLACEMENT_3D('',#2338,#1871,#1872);
#1619=AXIS2_PLACEMENT_3D('',#2340,#1874,#1875);
#1620=AXIS2_PLACEMENT_3D('',#2342,#1876,#1877);
#1621=AXIS2_PLACEMENT_3D('',#2344,#1878,#1879);
#1622=AXIS2_PLACEMENT_3D('',#2345,#1880,#1881);
#1623=AXIS2_PLACEMENT_3D('',#2348,#1883,#1884);
#1624=AXIS2_PLACEMENT_3D('',#2349,#1885,#1886);
#1625=AXIS2_PLACEMENT_3D('',#2351,#1887,#1888);
#1626=AXIS2_PLACEMENT_3D('',#2352,#1889,#1890);
#1627=AXIS2_PLACEMENT_3D('',#2354,#1891,#1892);
#1628=AXIS2_PLACEMENT_3D('',#2356,#1894,#1895);
#1629=AXIS2_PLACEMENT_3D('',#2358,#1896,#1897);
#1630=AXIS2_PLACEMENT_3D('',#2359,#1898,#1899);
#1631=AXIS2_PLACEMENT_3D('',#2361,#1900,#1901);
#1632=AXIS2_PLACEMENT_3D('',#2363,#1903,#1904);
#1633=AXIS2_PLACEMENT_3D('',#2366,#1906,#1907);
#1634=AXIS2_PLACEMENT_3D('',#2367,#1908,#1909);
#1635=AXIS2_PLACEMENT_3D('',#2369,#1910,#1911);
#1636=AXIS2_PLACEMENT_3D('',#2370,#1912,#1913);
#1637=AXIS2_PLACEMENT_3D('',#2372,#1915,#1916);
#1638=AXIS2_PLACEMENT_3D('',#2374,#1917,#1918);
#1639=AXIS2_PLACEMENT_3D('',#2375,#1919,#1920);
#1640=AXIS2_PLACEMENT_3D('',#2376,#1921,#1922);
#1641=AXIS2_PLACEMENT_3D('',#2378,#1923,#1924);
#1642=AXIS2_PLACEMENT_3D('',#2380,#1925,#1926);
#1643=AXIS2_PLACEMENT_3D('',#2381,#1927,#1928);
#1644=AXIS2_PLACEMENT_3D('',#2383,#1929,#1930);
#1645=AXIS2_PLACEMENT_3D('',#2385,#1932,#1933);
#1646=AXIS2_PLACEMENT_3D('',#2388,#1935,#1936);
#1647=AXIS2_PLACEMENT_3D('',#2389,#1937,#1938);
#1648=AXIS2_PLACEMENT_3D('',#2392,#1940,#1941);
#1649=AXIS2_PLACEMENT_3D('',#2393,#1942,#1943);
#1650=AXIS2_PLACEMENT_3D('',#2395,#1944,#1945);
#1651=AXIS2_PLACEMENT_3D('',#2396,#1946,#1947);
#1652=AXIS2_PLACEMENT_3D('',#2398,#1949,#1950);
#1653=AXIS2_PLACEMENT_3D('',#2400,#1951,#1952);
#1654=AXIS2_PLACEMENT_3D('',#2402,#1953,#1954);
#1655=AXIS2_PLACEMENT_3D('',#2403,#1955,#1956);
#1656=AXIS2_PLACEMENT_3D('',#2406,#1958,#1959);
#1657=AXIS2_PLACEMENT_3D('',#2407,#1960,#1961);
#1658=AXIS2_PLACEMENT_3D('',#2409,#1962,#1963);
#1659=AXIS2_PLACEMENT_3D('',#2410,#1964,#1965);
#1660=AXIS2_PLACEMENT_3D('',#2412,#1966,#1967);
#1661=AXIS2_PLACEMENT_3D('',#2414,#1969,#1970);
#1662=AXIS2_PLACEMENT_3D('',#2416,#1971,#1972);
#1663=AXIS2_PLACEMENT_3D('',#2417,#1973,#1974);
#1664=AXIS2_PLACEMENT_3D('',#2419,#1975,#1976);
#1665=AXIS2_PLACEMENT_3D('',#2421,#1978,#1979);
#1666=AXIS2_PLACEMENT_3D('',#2424,#1981,#1982);
#1667=AXIS2_PLACEMENT_3D('',#2425,#1983,#1984);
#1668=AXIS2_PLACEMENT_3D('',#2427,#1985,#1986);
#1669=AXIS2_PLACEMENT_3D('',#2428,#1987,#1988);
#1670=AXIS2_PLACEMENT_3D('',#2430,#1990,#1991);
#1671=AXIS2_PLACEMENT_3D('',#2432,#1992,#1993);
#1672=AXIS2_PLACEMENT_3D('',#2433,#1994,#1995);
#1673=AXIS2_PLACEMENT_3D('',#2434,#1996,#1997);
#1674=AXIS2_PLACEMENT_3D('',#2436,#1998,#1999);
#1675=AXIS2_PLACEMENT_3D('',#2438,#2000,#2001);
#1676=AXIS2_PLACEMENT_3D('',#2439,#2002,#2003);
#1677=AXIS2_PLACEMENT_3D('',#2441,#2004,#2005);
#1678=AXIS2_PLACEMENT_3D('',#2443,#2007,#2008);
#1679=AXIS2_PLACEMENT_3D('',#2446,#2010,#2011);
#1680=AXIS2_PLACEMENT_3D('',#2447,#2012,#2013);
#1681=AXIS2_PLACEMENT_3D('',#2450,#2015,#2016);
#1682=AXIS2_PLACEMENT_3D('',#2451,#2017,#2018);
#1683=AXIS2_PLACEMENT_3D('',#2453,#2019,#2020);
#1684=AXIS2_PLACEMENT_3D('',#2454,#2021,#2022);
#1685=AXIS2_PLACEMENT_3D('',#2456,#2024,#2025);
#1686=AXIS2_PLACEMENT_3D('',#2458,#2026,#2027);
#1687=AXIS2_PLACEMENT_3D('',#2460,#2028,#2029);
#1688=AXIS2_PLACEMENT_3D('',#2461,#2030,#2031);
#1689=AXIS2_PLACEMENT_3D('',#2464,#2033,#2034);
#1690=AXIS2_PLACEMENT_3D('',#2465,#2035,#2036);
#1691=AXIS2_PLACEMENT_3D('',#2467,#2037,#2038);
#1692=AXIS2_PLACEMENT_3D('',#2468,#2039,#2040);
#1693=AXIS2_PLACEMENT_3D('',#2470,#2041,#2042);
#1694=AXIS2_PLACEMENT_3D('',#2472,#2044,#2045);
#1695=AXIS2_PLACEMENT_3D('',#2474,#2046,#2047);
#1696=AXIS2_PLACEMENT_3D('',#2475,#2048,#2049);
#1697=AXIS2_PLACEMENT_3D('',#2477,#2050,#2051);
#1698=AXIS2_PLACEMENT_3D('',#2479,#2053,#2054);
#1699=AXIS2_PLACEMENT_3D('',#2482,#2056,#2057);
#1700=AXIS2_PLACEMENT_3D('',#2483,#2058,#2059);
#1701=AXIS2_PLACEMENT_3D('',#2485,#2060,#2061);
#1702=AXIS2_PLACEMENT_3D('',#2486,#2062,#2063);
#1703=AXIS2_PLACEMENT_3D('',#2488,#2065,#2066);
#1704=AXIS2_PLACEMENT_3D('',#2490,#2067,#2068);
#1705=AXIS2_PLACEMENT_3D('',#2491,#2069,#2070);
#1706=AXIS2_PLACEMENT_3D('',#2492,#2071,#2072);
#1707=AXIS2_PLACEMENT_3D('',#2495,#2073,#2074);
#1708=AXIS2_PLACEMENT_3D('',#2496,#2075,#2076);
#1709=AXIS2_PLACEMENT_3D('',#2497,#2077,#2078);
#1710=AXIS2_PLACEMENT_3D('',#2500,#2079,#2080);
#1711=AXIS2_PLACEMENT_3D('',#2501,#2081,#2082);
#1712=AXIS2_PLACEMENT_3D('',#2502,#2083,#2084);
#1713=AXIS2_PLACEMENT_3D('',#2505,#2085,#2086);
#1714=AXIS2_PLACEMENT_3D('',#2506,#2087,#2088);
#1715=AXIS2_PLACEMENT_3D('',#2507,#2089,#2090);
#1716=AXIS2_PLACEMENT_3D('',#2509,#2091,#2092);
#1717=AXIS2_PLACEMENT_3D('',#2512,#2094,#2095);
#1718=AXIS2_PLACEMENT_3D('',#2513,#2096,#2097);
#1719=AXIS2_PLACEMENT_3D('',#2537,#2109,#2110);
#1720=AXIS2_PLACEMENT_3D('',#2539,#2111,#2112);
#1721=AXIS2_PLACEMENT_3D('',#2540,#2113,#2114);
#1722=AXIS2_PLACEMENT_3D('',#2543,#2116,#2117);
#1723=AXIS2_PLACEMENT_3D('',#2544,#2118,#2119);
#1724=AXIS2_PLACEMENT_3D('',#2546,#2120,#2121);
#1725=AXIS2_PLACEMENT_3D('',#2548,#2123,#2124);
#1726=AXIS2_PLACEMENT_3D('',#2551,#2126,#2127);
#1727=AXIS2_PLACEMENT_3D('',#2552,#2128,#2129);
#1728=AXIS2_PLACEMENT_3D('',#2558,#2133,#2134);
#1729=AXIS2_PLACEMENT_3D('',#2562,#2137,#2138);
#1730=AXIS2_PLACEMENT_3D('',#2566,#2141,#2142);
#1731=AXIS2_PLACEMENT_3D('',#2570,#2145,#2146);
#1732=AXIS2_PLACEMENT_3D('',#2576,#2150,#2151);
#1733=AXIS2_PLACEMENT_3D('',#2580,#2154,#2155);
#1734=AXIS2_PLACEMENT_3D('',#2584,#2158,#2159);
#1735=AXIS2_PLACEMENT_3D('',#2588,#2162,#2163);
#1736=AXIS2_PLACEMENT_3D('',#2603,#2171,#2172);
#1737=AXIS2_PLACEMENT_3D('',#2604,#2173,#2174);
#1738=AXIS2_PLACEMENT_3D('',#2608,#2177,#2178);
#1739=AXIS2_PLACEMENT_3D('',#2614,#2182,#2183);
#1740=AXIS2_PLACEMENT_3D('',#2618,#2186,#2187);
#1741=AXIS2_PLACEMENT_3D('',#2622,#2190,#2191);
#1742=AXIS2_PLACEMENT_3D('',#2626,#2194,#2195);
#1743=AXIS2_PLACEMENT_3D('',#2628,#2197,#2198);
#1744=AXIS2_PLACEMENT_3D('',#2630,#2200,#2201);
#1745=AXIS2_PLACEMENT_3D('',#2632,#2203,#2204);
#1746=AXIS2_PLACEMENT_3D('',#2634,#2206,#2207);
#1747=AXIS2_PLACEMENT_3D('',#2636,#2209,#2210);
#1748=AXIS2_PLACEMENT_3D('',#2638,#2212,#2213);
#1749=AXIS2_PLACEMENT_3D('',#2640,#2215,#2216);
#1750=AXIS2_PLACEMENT_3D('',#2642,#2218,#2219);
#1751=AXIS2_PLACEMENT_3D('',#2643,#2220,#2221);
#1752=AXIS2_PLACEMENT_3D('',#2645,#2222,#2223);
#1753=AXIS2_PLACEMENT_3D('',#2647,#2225,#2226);
#1754=AXIS2_PLACEMENT_3D('',#2649,#2228,#2229);
#1755=AXIS2_PLACEMENT_3D('',#2650,#2230,#2231);
#1756=AXIS2_PLACEMENT_3D('',#2651,#2232,#2233);
#1757=AXIS2_PLACEMENT_3D('',#2652,#2234,#2235);
#1758=AXIS2_PLACEMENT_3D('',#2653,#2236,#2237);
#1759=AXIS2_PLACEMENT_3D('',#2654,#2238,#2239);
#1760=AXIS2_PLACEMENT_3D('',#2655,#2240,#2241);
#1761=AXIS2_PLACEMENT_3D('',#2656,#2242,#2243);
#1762=DIRECTION('axis',(0.,0.,1.));
#1763=DIRECTION('refdir',(1.,0.,0.));
#1764=DIRECTION('axis',(0.,0.,1.));
#1765=DIRECTION('refdir',(1.,0.,0.));
#1766=DIRECTION('center_axis',(0.,0.,1.));
#1767=DIRECTION('ref_axis',(-1.,0.,0.));
#1768=DIRECTION('center_axis',(0.,0.,-1.));
#1769=DIRECTION('ref_axis',(-1.,0.,0.));
#1770=DIRECTION('',(0.707106781186548,8.65956056235494E-17,0.707106781186547));
#1771=DIRECTION('center_axis',(0.,0.,1.));
#1772=DIRECTION('ref_axis',(-1.,0.,0.));
#1773=DIRECTION('center_axis',(0.,0.,1.));
#1774=DIRECTION('ref_axis',(1.,0.,0.));
#1775=DIRECTION('',(0.,-1.,0.));
#1776=DIRECTION('',(1.,0.,0.));
#1777=DIRECTION('',(0.,1.,0.));
#1778=DIRECTION('',(-1.,0.,0.));
#1779=DIRECTION('',(-0.707106781186547,-0.707106781186547,0.));
#1780=DIRECTION('center_axis',(0.,0.,1.));
#1781=DIRECTION('ref_axis',(-1.,0.,0.));
#1782=DIRECTION('center_axis',(0.,0.,-1.));
#1783=DIRECTION('ref_axis',(1.,0.,0.));
#1784=DIRECTION('center_axis',(0.,0.,1.));
#1785=DIRECTION('ref_axis',(-1.,0.,0.));
#1786=DIRECTION('center_axis',(0.,0.,-1.));
#1787=DIRECTION('ref_axis',(-1.,0.,0.));
#1788=DIRECTION('',(0.,0.,-1.));
#1789=DIRECTION('center_axis',(0.,0.,-1.));
#1790=DIRECTION('ref_axis',(-1.,0.,0.));
#1791=DIRECTION('center_axis',(0.,0.,1.));
#1792=DIRECTION('ref_axis',(-1.,0.,0.));
#1793=DIRECTION('center_axis',(0.,0.,-1.));
#1794=DIRECTION('ref_axis',(-1.,0.,0.));
#1795=DIRECTION('',(0.707106781186548,8.65956056235494E-17,0.707106781186547));
#1796=DIRECTION('center_axis',(0.,0.,-1.));
#1797=DIRECTION('ref_axis',(-1.,0.,0.));
#1798=DIRECTION('',(0.,0.,-1.));
#1799=DIRECTION('center_axis',(0.,0.,-1.));
#1800=DIRECTION('ref_axis',(-1.,0.,0.));
#1801=DIRECTION('center_axis',(0.,0.,1.));
#1802=DIRECTION('ref_axis',(-1.,0.,0.));
#1803=DIRECTION('center_axis',(0.,0.,-1.));
#1804=DIRECTION('ref_axis',(-1.,0.,0.));
#1805=DIRECTION('',(0.707106781186548,8.65956056235494E-17,0.707106781186547));
#1806=DIRECTION('center_axis',(0.,0.,-1.));
#1807=DIRECTION('ref_axis',(-1.,0.,0.));
#1808=DIRECTION('',(0.,0.,-1.));
#1809=DIRECTION('center_axis',(0.,0.,-1.));
#1810=DIRECTION('ref_axis',(-1.,0.,0.));
#1811=DIRECTION('center_axis',(0.,0.,1.));
#1812=DIRECTION('ref_axis',(-1.,0.,0.));
#1813=DIRECTION('center_axis',(0.,0.,1.));
#1814=DIRECTION('ref_axis',(-1.,0.,0.));
#1815=DIRECTION('center_axis',(0.,0.,1.));
#1816=DIRECTION('ref_axis',(-1.,0.,0.));
#1817=DIRECTION('center_axis',(0.,0.,1.));
#1818=DIRECTION('ref_axis',(1.,0.,0.));
#1819=DIRECTION('center_axis',(0.,0.,-1.));
#1820=DIRECTION('ref_axis',(1.,0.,0.));
#1821=DIRECTION('',(0.,0.,1.));
#1822=DIRECTION('center_axis',(-0.707106781186548,0.707106781186548,0.));
#1823=DIRECTION('ref_axis',(-0.707106781186548,-0.707106781186548,0.));
#1824=DIRECTION('',(0.707106781186547,0.707106781186547,0.));
#1825=DIRECTION('',(0.,0.,1.));
#1826=DIRECTION('',(0.,0.,1.));
#1827=DIRECTION('center_axis',(0.,1.,0.));
#1828=DIRECTION('ref_axis',(-1.,0.,0.));
#1829=DIRECTION('',(-1.,0.,0.));
#1830=DIRECTION('',(0.,0.,1.));
#1831=DIRECTION('center_axis',(1.,0.,0.));
#1832=DIRECTION('ref_axis',(0.,1.,0.));
#1833=DIRECTION('',(0.,1.,0.));
#1834=DIRECTION('',(0.,0.,1.));
#1835=DIRECTION('center_axis',(0.,-1.,0.));
#1836=DIRECTION('ref_axis',(1.,0.,0.));
#1837=DIRECTION('',(1.,0.,0.));
#1838=DIRECTION('',(0.,0.,1.));
#1839=DIRECTION('center_axis',(-1.,0.,0.));
#1840=DIRECTION('ref_axis',(0.,-1.,0.));
#1841=DIRECTION('',(0.,-1.,0.));
#1842=DIRECTION('center_axis',(0.,0.,1.));
#1843=DIRECTION('ref_axis',(1.,0.,0.));
#1844=DIRECTION('axis',(0.,0.,1.));
#1845=DIRECTION('refdir',(1.,0.,0.));
#1846=DIRECTION('center_axis',(0.,0.,1.));
#1847=DIRECTION('ref_axis',(-1.,0.,0.));
#1848=DIRECTION('center_axis',(0.,0.,-1.));
#1849=DIRECTION('ref_axis',(-1.,0.,0.));
#1850=DIRECTION('center_axis',(0.,0.,1.));
#1851=DIRECTION('ref_axis',(-1.,0.,0.));
#1852=DIRECTION('center_axis',(0.,0.,-1.));
#1853=DIRECTION('ref_axis',(-1.,0.,0.));
#1854=DIRECTION('center_axis',(0.,0.,-1.));
#1855=DIRECTION('ref_axis',(-1.,0.,0.));
#1856=DIRECTION('',(0.,0.,-1.));
#1857=DIRECTION('center_axis',(0.,0.,1.));
#1858=DIRECTION('ref_axis',(-1.,0.,0.));
#1859=DIRECTION('',(0.707106781186547,8.65956056235493E-17,0.707106781186548));
#1860=DIRECTION('center_axis',(0.,0.,1.));
#1861=DIRECTION('ref_axis',(-1.,0.,0.));
#1862=DIRECTION('center_axis',(0.,0.,-1.));
#1863=DIRECTION('ref_axis',(-1.,0.,0.));
#1864=DIRECTION('',(0.,0.,1.));
#1865=DIRECTION('center_axis',(0.,0.,1.));
#1866=DIRECTION('ref_axis',(-1.,0.,0.));
#1867=DIRECTION('center_axis',(0.,0.,1.));
#1868=DIRECTION('ref_axis',(-1.,0.,0.));
#1869=DIRECTION('center_axis',(0.,0.,-1.));
#1870=DIRECTION('ref_axis',(-1.,0.,0.));
#1871=DIRECTION('center_axis',(0.,0.,-1.));
#1872=DIRECTION('ref_axis',(-1.,0.,0.));
#1873=DIRECTION('',(-0.707106781186547,8.65956056235493E-17,0.707106781186548));
#1874=DIRECTION('center_axis',(0.,0.,1.));
#1875=DIRECTION('ref_axis',(-1.,0.,0.));
#1876=DIRECTION('center_axis',(0.,0.,-1.));
#1877=DIRECTION('ref_axis',(-1.,0.,0.));
#1878=DIRECTION('center_axis',(0.,0.,1.));
#1879=DIRECTION('ref_axis',(0.,-1.,0.));
#1880=DIRECTION('center_axis',(0.,0.,-1.));
#1881=DIRECTION('ref_axis',(-1.,0.,0.));
#1882=DIRECTION('',(0.,0.,1.));
#1883=DIRECTION('center_axis',(0.,0.,-1.));
#1884=DIRECTION('ref_axis',(-1.,0.,0.));
#1885=DIRECTION('center_axis',(0.,0.,1.));
#1886=DIRECTION('ref_axis',(-1.,0.,0.));
#1887=DIRECTION('center_axis',(0.,0.,1.));
#1888=DIRECTION('ref_axis',(-1.,0.,0.));
#1889=DIRECTION('center_axis',(0.,0.,-1.));
#1890=DIRECTION('ref_axis',(-1.,0.,0.));
#1891=DIRECTION('center_axis',(0.,0.,1.));
#1892=DIRECTION('ref_axis',(-1.,0.,0.));
#1893=DIRECTION('',(0.,0.,1.));
#1894=DIRECTION('center_axis',(0.,0.,1.));
#1895=DIRECTION('ref_axis',(-1.,0.,0.));
#1896=DIRECTION('center_axis',(0.,0.,-1.));
#1897=DIRECTION('ref_axis',(-1.,0.,0.));
#1898=DIRECTION('center_axis',(0.,0.,-1.));
#1899=DIRECTION('ref_axis',(-1.,0.,0.));
#1900=DIRECTION('center_axis',(0.,0.,-1.));
#1901=DIRECTION('ref_axis',(-1.,0.,0.));
#1902=DIRECTION('',(0.,0.,1.));
#1903=DIRECTION('center_axis',(0.,0.,1.));
#1904=DIRECTION('ref_axis',(-1.,0.,0.));
#1905=DIRECTION('',(-0.707106781186547,-8.65956056235493E-17,-0.707106781186548));
#1906=DIRECTION('center_axis',(0.,0.,1.));
#1907=DIRECTION('ref_axis',(-1.,0.,0.));
#1908=DIRECTION('center_axis',(0.,0.,1.));
#1909=DIRECTION('ref_axis',(-1.,0.,0.));
#1910=DIRECTION('center_axis',(0.,0.,-1.));
#1911=DIRECTION('ref_axis',(-1.,0.,0.));
#1912=DIRECTION('center_axis',(0.,0.,-1.));
#1913=DIRECTION('ref_axis',(-1.,0.,0.));
#1914=DIRECTION('',(0.707106781186547,-8.65956056235493E-17,-0.707106781186548));
#1915=DIRECTION('center_axis',(0.,0.,1.));
#1916=DIRECTION('ref_axis',(1.,0.,0.));
#1917=DIRECTION('center_axis',(0.,1.,0.));
#1918=DIRECTION('ref_axis',(-1.,0.,0.));
#1919=DIRECTION('axis',(0.,0.,1.));
#1920=DIRECTION('refdir',(1.,0.,0.));
#1921=DIRECTION('center_axis',(0.,0.,1.));
#1922=DIRECTION('ref_axis',(-1.,0.,0.));
#1923=DIRECTION('center_axis',(0.,0.,-1.));
#1924=DIRECTION('ref_axis',(-1.,0.,0.));
#1925=DIRECTION('center_axis',(0.,0.,1.));
#1926=DIRECTION('ref_axis',(-1.,0.,0.));
#1927=DIRECTION('center_axis',(0.,0.,-1.));
#1928=DIRECTION('ref_axis',(-1.,0.,0.));
#1929=DIRECTION('center_axis',(0.,0.,-1.));
#1930=DIRECTION('ref_axis',(-1.,0.,0.));
#1931=DIRECTION('',(0.,0.,-1.));
#1932=DIRECTION('center_axis',(0.,0.,1.));
#1933=DIRECTION('ref_axis',(-1.,0.,0.));
#1934=DIRECTION('',(0.707106781186547,8.65956056235493E-17,0.707106781186548));
#1935=DIRECTION('center_axis',(0.,0.,1.));
#1936=DIRECTION('ref_axis',(-1.,0.,0.));
#1937=DIRECTION('center_axis',(0.,0.,-1.));
#1938=DIRECTION('ref_axis',(-1.,0.,0.));
#1939=DIRECTION('',(0.,0.,1.));
#1940=DIRECTION('center_axis',(0.,0.,1.));
#1941=DIRECTION('ref_axis',(-1.,0.,0.));
#1942=DIRECTION('center_axis',(0.,0.,1.));
#1943=DIRECTION('ref_axis',(-1.,0.,0.));
#1944=DIRECTION('center_axis',(0.,0.,-1.));
#1945=DIRECTION('ref_axis',(-1.,0.,0.));
#1946=DIRECTION('center_axis',(0.,0.,-1.));
#1947=DIRECTION('ref_axis',(-1.,0.,0.));
#1948=DIRECTION('',(-0.707106781186547,8.65956056235493E-17,0.707106781186548));
#1949=DIRECTION('center_axis',(0.,0.,1.));
#1950=DIRECTION('ref_axis',(-1.,0.,0.));
#1951=DIRECTION('center_axis',(0.,0.,-1.));
#1952=DIRECTION('ref_axis',(-1.,0.,0.));
#1953=DIRECTION('center_axis',(0.,0.,1.));
#1954=DIRECTION('ref_axis',(0.,-1.,0.));
#1955=DIRECTION('center_axis',(0.,0.,-1.));
#1956=DIRECTION('ref_axis',(-1.,0.,0.));
#1957=DIRECTION('',(0.,0.,1.));
#1958=DIRECTION('center_axis',(0.,0.,-1.));
#1959=DIRECTION('ref_axis',(-1.,0.,0.));
#1960=DIRECTION('center_axis',(0.,0.,1.));
#1961=DIRECTION('ref_axis',(-1.,0.,0.));
#1962=DIRECTION('center_axis',(0.,0.,1.));
#1963=DIRECTION('ref_axis',(-1.,0.,0.));
#1964=DIRECTION('center_axis',(0.,0.,-1.));
#1965=DIRECTION('ref_axis',(-1.,0.,0.));
#1966=DIRECTION('center_axis',(0.,0.,1.));
#1967=DIRECTION('ref_axis',(-1.,0.,0.));
#1968=DIRECTION('',(0.,0.,1.));
#1969=DIRECTION('center_axis',(0.,0.,1.));
#1970=DIRECTION('ref_axis',(-1.,0.,0.));
#1971=DIRECTION('center_axis',(0.,0.,-1.));
#1972=DIRECTION('ref_axis',(-1.,0.,0.));
#1973=DIRECTION('center_axis',(0.,0.,-1.));
#1974=DIRECTION('ref_axis',(-1.,0.,0.));
#1975=DIRECTION('center_axis',(0.,0.,-1.));
#1976=DIRECTION('ref_axis',(-1.,0.,0.));
#1977=DIRECTION('',(0.,0.,1.));
#1978=DIRECTION('center_axis',(0.,0.,1.));
#1979=DIRECTION('ref_axis',(-1.,0.,0.));
#1980=DIRECTION('',(-0.707106781186547,-8.65956056235493E-17,-0.707106781186548));
#1981=DIRECTION('center_axis',(0.,0.,1.));
#1982=DIRECTION('ref_axis',(-1.,0.,0.));
#1983=DIRECTION('center_axis',(0.,0.,1.));
#1984=DIRECTION('ref_axis',(-1.,0.,0.));
#1985=DIRECTION('center_axis',(0.,0.,-1.));
#1986=DIRECTION('ref_axis',(-1.,0.,0.));
#1987=DIRECTION('center_axis',(0.,0.,-1.));
#1988=DIRECTION('ref_axis',(-1.,0.,0.));
#1989=DIRECTION('',(0.707106781186547,-8.65956056235493E-17,-0.707106781186548));
#1990=DIRECTION('center_axis',(0.,0.,1.));
#1991=DIRECTION('ref_axis',(1.,0.,0.));
#1992=DIRECTION('center_axis',(0.,1.,0.));
#1993=DIRECTION('ref_axis',(-1.,0.,0.));
#1994=DIRECTION('axis',(0.,0.,1.));
#1995=DIRECTION('refdir',(1.,0.,0.));
#1996=DIRECTION('center_axis',(0.,0.,1.));
#1997=DIRECTION('ref_axis',(-1.,0.,0.));
#1998=DIRECTION('center_axis',(0.,0.,-1.));
#1999=DIRECTION('ref_axis',(-1.,0.,0.));
#2000=DIRECTION('center_axis',(0.,0.,1.));
#2001=DIRECTION('ref_axis',(-1.,0.,0.));
#2002=DIRECTION('center_axis',(0.,0.,-1.));
#2003=DIRECTION('ref_axis',(-1.,0.,0.));
#2004=DIRECTION('center_axis',(0.,0.,-1.));
#2005=DIRECTION('ref_axis',(-1.,0.,0.));
#2006=DIRECTION('',(0.,0.,-1.));
#2007=DIRECTION('center_axis',(0.,0.,1.));
#2008=DIRECTION('ref_axis',(-1.,0.,0.));
#2009=DIRECTION('',(0.707106781186547,8.65956056235493E-17,0.707106781186548));
#2010=DIRECTION('center_axis',(0.,0.,1.));
#2011=DIRECTION('ref_axis',(-1.,0.,0.));
#2012=DIRECTION('center_axis',(0.,0.,-1.));
#2013=DIRECTION('ref_axis',(-1.,0.,0.));
#2014=DIRECTION('',(0.,0.,1.));
#2015=DIRECTION('center_axis',(0.,0.,1.));
#2016=DIRECTION('ref_axis',(-1.,0.,0.));
#2017=DIRECTION('center_axis',(0.,0.,1.));
#2018=DIRECTION('ref_axis',(-1.,0.,0.));
#2019=DIRECTION('center_axis',(0.,0.,-1.));
#2020=DIRECTION('ref_axis',(-1.,0.,0.));
#2021=DIRECTION('center_axis',(0.,0.,-1.));
#2022=DIRECTION('ref_axis',(-1.,0.,0.));
#2023=DIRECTION('',(-0.707106781186547,8.65956056235493E-17,0.707106781186548));
#2024=DIRECTION('center_axis',(0.,0.,1.));
#2025=DIRECTION('ref_axis',(-1.,0.,0.));
#2026=DIRECTION('center_axis',(0.,0.,-1.));
#2027=DIRECTION('ref_axis',(-1.,0.,0.));
#2028=DIRECTION('center_axis',(0.,0.,1.));
#2029=DIRECTION('ref_axis',(0.,-1.,0.));
#2030=DIRECTION('center_axis',(0.,0.,-1.));
#2031=DIRECTION('ref_axis',(-1.,0.,0.));
#2032=DIRECTION('',(0.,0.,1.));
#2033=DIRECTION('center_axis',(0.,0.,-1.));
#2034=DIRECTION('ref_axis',(-1.,0.,0.));
#2035=DIRECTION('center_axis',(0.,0.,1.));
#2036=DIRECTION('ref_axis',(-1.,0.,0.));
#2037=DIRECTION('center_axis',(0.,0.,1.));
#2038=DIRECTION('ref_axis',(-1.,0.,0.));
#2039=DIRECTION('center_axis',(0.,0.,-1.));
#2040=DIRECTION('ref_axis',(-1.,0.,0.));
#2041=DIRECTION('center_axis',(0.,0.,1.));
#2042=DIRECTION('ref_axis',(-1.,0.,0.));
#2043=DIRECTION('',(0.,0.,1.));
#2044=DIRECTION('center_axis',(0.,0.,1.));
#2045=DIRECTION('ref_axis',(-1.,0.,0.));
#2046=DIRECTION('center_axis',(0.,0.,-1.));
#2047=DIRECTION('ref_axis',(-1.,0.,0.));
#2048=DIRECTION('center_axis',(0.,0.,-1.));
#2049=DIRECTION('ref_axis',(-1.,0.,0.));
#2050=DIRECTION('center_axis',(0.,0.,-1.));
#2051=DIRECTION('ref_axis',(-1.,0.,0.));
#2052=DIRECTION('',(0.,0.,1.));
#2053=DIRECTION('center_axis',(0.,0.,1.));
#2054=DIRECTION('ref_axis',(-1.,0.,0.));
#2055=DIRECTION('',(-0.707106781186547,-8.65956056235493E-17,-0.707106781186548));
#2056=DIRECTION('center_axis',(0.,0.,1.));
#2057=DIRECTION('ref_axis',(-1.,0.,0.));
#2058=DIRECTION('center_axis',(0.,0.,1.));
#2059=DIRECTION('ref_axis',(-1.,0.,0.));
#2060=DIRECTION('center_axis',(0.,0.,-1.));
#2061=DIRECTION('ref_axis',(-1.,0.,0.));
#2062=DIRECTION('center_axis',(0.,0.,-1.));
#2063=DIRECTION('ref_axis',(-1.,0.,0.));
#2064=DIRECTION('',(0.707106781186547,-8.65956056235493E-17,-0.707106781186548));
#2065=DIRECTION('center_axis',(0.,0.,1.));
#2066=DIRECTION('ref_axis',(1.,0.,0.));
#2067=DIRECTION('center_axis',(0.,1.,0.));
#2068=DIRECTION('ref_axis',(-1.,0.,0.));
#2069=DIRECTION('axis',(0.,0.,1.));
#2070=DIRECTION('refdir',(1.,0.,0.));
#2071=DIRECTION('center_axis',(0.,0.,1.));
#2072=DIRECTION('ref_axis',(1.,0.,0.));
#2073=DIRECTION('center_axis',(0.,-1.,0.));
#2074=DIRECTION('ref_axis',(-1.,0.,0.));
#2075=DIRECTION('axis',(0.,0.,1.));
#2076=DIRECTION('refdir',(1.,0.,0.));
#2077=DIRECTION('center_axis',(0.,0.,1.));
#2078=DIRECTION('ref_axis',(1.,0.,0.));
#2079=DIRECTION('center_axis',(0.,-1.,0.));
#2080=DIRECTION('ref_axis',(-1.,0.,0.));
#2081=DIRECTION('axis',(0.,0.,1.));
#2082=DIRECTION('refdir',(1.,0.,0.));
#2083=DIRECTION('center_axis',(0.,0.,1.));
#2084=DIRECTION('ref_axis',(-1.,0.,0.));
#2085=DIRECTION('center_axis',(0.,1.,0.));
#2086=DIRECTION('ref_axis',(1.,0.,0.));
#2087=DIRECTION('axis',(0.,0.,1.));
#2088=DIRECTION('refdir',(1.,0.,0.));
#2089=DIRECTION('center_axis',(0.,0.,1.));
#2090=DIRECTION('ref_axis',(-1.,0.,0.));
#2091=DIRECTION('center_axis',(0.,0.,-1.));
#2092=DIRECTION('ref_axis',(-1.,0.,0.));
#2093=DIRECTION('',(0.707106781186547,8.65956056235493E-17,0.707106781186548));
#2094=DIRECTION('center_axis',(0.,0.,1.));
#2095=DIRECTION('ref_axis',(-1.,0.,0.));
#2096=DIRECTION('center_axis',(0.,0.,1.));
#2097=DIRECTION('ref_axis',(1.,0.,0.));
#2098=DIRECTION('',(-0.707106781186548,0.707106781186547,0.));
#2099=DIRECTION('',(-1.,0.,0.));
#2100=DIRECTION('',(-0.707106781186548,-0.707106781186547,0.));
#2101=DIRECTION('',(0.,-1.,0.));
#2102=DIRECTION('',(0.707106781186547,-0.707106781186547,0.));
#2103=DIRECTION('',(1.,0.,0.));
#2104=DIRECTION('',(0.707106781186547,0.707106781186548,0.));
#2105=DIRECTION('',(0.,1.,0.));
#2106=DIRECTION('',(1.,0.,0.));
#2107=DIRECTION('',(0.707106781186548,0.707106781186547,0.));
#2108=DIRECTION('',(0.,1.,0.));
#2109=DIRECTION('center_axis',(0.,0.,1.));
#2110=DIRECTION('ref_axis',(-1.,0.,0.));
#2111=DIRECTION('center_axis',(0.,0.,1.));
#2112=DIRECTION('ref_axis',(-1.,0.,0.));
#2113=DIRECTION('center_axis',(0.,0.,-1.));
#2114=DIRECTION('ref_axis',(-1.,0.,0.));
#2115=DIRECTION('',(0.,0.,-1.));
#2116=DIRECTION('center_axis',(0.,0.,1.));
#2117=DIRECTION('ref_axis',(-1.,0.,0.));
#2118=DIRECTION('center_axis',(0.,0.,1.));
#2119=DIRECTION('ref_axis',(-1.,0.,0.));
#2120=DIRECTION('center_axis',(0.,0.,-1.));
#2121=DIRECTION('ref_axis',(-1.,0.,0.));
#2122=DIRECTION('',(0.707106781186547,8.65956056235493E-17,0.707106781186548));
#2123=DIRECTION('center_axis',(0.,0.,-1.));
#2124=DIRECTION('ref_axis',(-1.,0.,0.));
#2125=DIRECTION('',(0.,0.,-1.));
#2126=DIRECTION('center_axis',(0.,0.,1.));
#2127=DIRECTION('ref_axis',(-1.,0.,0.));
#2128=DIRECTION('center_axis',(-0.500000000000001,-0.500000000000001,0.707106781186546));
#2129=DIRECTION('ref_axis',(0.816496580927725,-1.47935320064922E-16,0.577350269189627));
#2130=DIRECTION('',(0.707106781186548,-0.707106781186547,0.));
#2131=DIRECTION('',(0.281084637714816,0.678598344545848,0.678598344545848));
#2132=DIRECTION('',(-0.678598344545848,-0.281084637714818,-0.678598344545848));
#2133=DIRECTION('center_axis',(-0.707106781186548,0.,0.707106781186548));
#2134=DIRECTION('ref_axis',(0.707106781186548,0.,0.707106781186548));
#2135=DIRECTION('',(-0.678598344545847,0.281084637714821,-0.678598344545847));
#2136=DIRECTION('',(0.,-1.,0.));
#2137=DIRECTION('center_axis',(-0.5,0.500000000000001,0.707106781186547));
#2138=DIRECTION('ref_axis',(0.816496580927726,1.11022302462516E-16,0.577350269189626));
#2139=DIRECTION('',(-0.281084637714819,0.678598344545847,-0.678598344545848));
#2140=DIRECTION('',(-0.707106781186548,-0.707106781186547,0.));
#2141=DIRECTION('center_axis',(0.,0.707106781186548,0.707106781186547));
#2142=DIRECTION('ref_axis',(1.,0.,0.));
#2143=DIRECTION('',(0.577350269189626,-0.577350269189625,0.577350269189626));
#2144=DIRECTION('',(-1.,0.,0.));
#2145=DIRECTION('center_axis',(-0.707106781186547,-0.707106781186548,0.));
#2146=DIRECTION('ref_axis',(0.,0.,1.));
#2147=DIRECTION('',(0.,0.,-1.));
#2148=DIRECTION('',(0.707106781186548,-0.707106781186547,0.));
#2149=DIRECTION('',(0.,0.,1.));
#2150=DIRECTION('center_axis',(-1.,0.,0.));
#2151=DIRECTION('ref_axis',(0.,-1.,0.));
#2152=DIRECTION('',(0.,0.,1.));
#2153=DIRECTION('',(0.,-1.,0.));
#2154=DIRECTION('center_axis',(-0.707106781186547,0.707106781186549,0.));
#2155=DIRECTION('ref_axis',(0.,0.,1.));
#2156=DIRECTION('',(0.,0.,-1.));
#2157=DIRECTION('',(-0.707106781186548,-0.707106781186547,0.));
#2158=DIRECTION('center_axis',(0.,1.,0.));
#2159=DIRECTION('ref_axis',(-1.,0.,0.));
#2160=DIRECTION('',(0.,0.,1.));
#2161=DIRECTION('',(1.,0.,0.));
#2162=DIRECTION('center_axis',(0.,0.,1.));
#2163=DIRECTION('ref_axis',(1.,0.,0.));
#2164=DIRECTION('',(0.,-1.,0.));
#2165=DIRECTION('',(-0.707106781186547,-0.707106781186548,0.));
#2166=DIRECTION('',(1.,0.,0.));
#2167=DIRECTION('',(-0.707106781186547,0.707106781186547,0.));
#2168=DIRECTION('',(0.,1.,0.));
#2169=DIRECTION('',(0.707106781186548,0.707106781186547,0.));
#2170=DIRECTION('',(-1.,0.,0.));
#2171=DIRECTION('center_axis',(0.,0.,1.));
#2172=DIRECTION('ref_axis',(-1.,0.,0.));
#2173=DIRECTION('center_axis',(-0.707106781186548,0.,0.707106781186548));
#2174=DIRECTION('ref_axis',(0.707106781186548,0.,0.707106781186548));
#2175=DIRECTION('',(0.,-1.,0.));
#2176=DIRECTION('',(-0.678598344545848,0.281084637714819,-0.678598344545847));
#2177=DIRECTION('center_axis',(0.,0.707106781186548,0.707106781186548));
#2178=DIRECTION('ref_axis',(1.,0.,0.));
#2179=DIRECTION('',(0.281084637714818,0.678598344545848,-0.678598344545848));
#2180=DIRECTION('',(-1.,0.,0.));
#2181=DIRECTION('',(0.281084637714822,-0.678598344545847,0.678598344545847));
#2182=DIRECTION('center_axis',(0.500000000000001,0.500000000000001,0.707106781186547));
#2183=DIRECTION('ref_axis',(0.816496580927725,1.16630067516701E-16,-0.577350269189627));
#2184=DIRECTION('',(0.678598344545847,0.281084637714819,-0.678598344545847));
#2185=DIRECTION('',(-0.707106781186547,0.707106781186547,0.));
#2186=DIRECTION('center_axis',(0.707106781186548,0.,0.707106781186548));
#2187=DIRECTION('ref_axis',(0.707106781186548,0.,-0.707106781186548));
#2188=DIRECTION('',(0.678598344545847,-0.281084637714821,-0.678598344545847));
#2189=DIRECTION('',(0.,1.,0.));
#2190=DIRECTION('center_axis',(0.5,-0.500000000000001,0.707106781186547));
#2191=DIRECTION('ref_axis',(0.816496580927726,1.11022302462516E-16,-0.577350269189626));
#2192=DIRECTION('',(0.281084637714819,-0.678598344545847,-0.678598344545847));
#2193=DIRECTION('',(0.707106781186548,0.707106781186547,0.));
#2194=DIRECTION('center_axis',(0.,-0.707106781186548,0.707106781186548));
#2195=DIRECTION('ref_axis',(1.,0.,0.));
#2196=DIRECTION('',(1.,0.,0.));
#2197=DIRECTION('center_axis',(-0.500000000000001,0.5,0.707106781186547));
#2198=DIRECTION('ref_axis',(0.816496580927725,-1.19433950043794E-16,0.577350269189627));
#2199=DIRECTION('',(-0.707106781186547,-0.707106781186548,0.));
#2200=DIRECTION('center_axis',(-1.,0.,0.));
#2201=DIRECTION('ref_axis',(0.,-1.,0.));
#2202=DIRECTION('',(0.,0.,1.));
#2203=DIRECTION('center_axis',(-0.707106781186548,0.707106781186547,0.));
#2204=DIRECTION('ref_axis',(0.,0.,1.));
#2205=DIRECTION('',(0.,0.,-1.));
#2206=DIRECTION('center_axis',(0.,1.,0.));
#2207=DIRECTION('ref_axis',(-1.,0.,0.));
#2208=DIRECTION('',(0.,0.,1.));
#2209=DIRECTION('center_axis',(0.707106781186548,0.707106781186548,0.));
#2210=DIRECTION('ref_axis',(0.,0.,-1.));
#2211=DIRECTION('',(0.,0.,-1.));
#2212=DIRECTION('center_axis',(1.,0.,0.));
#2213=DIRECTION('ref_axis',(0.,1.,0.));
#2214=DIRECTION('',(0.,0.,1.));
#2215=DIRECTION('center_axis',(0.707106781186547,-0.707106781186548,0.));
#2216=DIRECTION('ref_axis',(0.,0.,-1.));
#2217=DIRECTION('',(0.,0.,-1.));
#2218=DIRECTION('center_axis',(0.,-1.,0.));
#2219=DIRECTION('ref_axis',(1.,0.,0.));
#2220=DIRECTION('center_axis',(0.,0.,1.));
#2221=DIRECTION('ref_axis',(-1.,0.,0.));
#2222=DIRECTION('center_axis',(0.,0.,-1.));
#2223=DIRECTION('ref_axis',(-1.,0.,0.));
#2224=DIRECTION('',(0.707106781186547,8.65956056235493E-17,0.707106781186548));
#2225=DIRECTION('center_axis',(0.,0.,-1.));
#2226=DIRECTION('ref_axis',(-1.,0.,0.));
#2227=DIRECTION('',(0.,0.,-1.));
#2228=DIRECTION('',(0.,0.,1.));
#2229=DIRECTION('',(1.,0.,0.));
#2230=DIRECTION('',(0.,0.,1.));
#2231=DIRECTION('',(1.,0.,0.));
#2232=DIRECTION('',(0.,0.,1.));
#2233=DIRECTION('',(1.,0.,0.));
#2234=DIRECTION('',(0.,0.,1.));
#2235=DIRECTION('',(1.,0.,0.));
#2236=DIRECTION('',(0.,0.,1.));
#2237=DIRECTION('',(1.,0.,0.));
#2238=DIRECTION('',(0.,0.,1.));
#2239=DIRECTION('',(1.,0.,0.));
#2240=DIRECTION('',(0.,0.,1.));
#2241=DIRECTION('',(1.,0.,0.));
#2242=DIRECTION('',(0.,0.,1.));
#2243=DIRECTION('',(1.,0.,0.));
#2244=CARTESIAN_POINT('',(0.,0.,0.));
#2245=CARTESIAN_POINT('',(0.,0.,0.));
#2246=CARTESIAN_POINT('Origin',(-8.,-7.5,3.75));
#2247=CARTESIAN_POINT('',(-6.,-7.5,3.5));
#2248=CARTESIAN_POINT('Origin',(-8.,-7.5,3.5));
#2249=CARTESIAN_POINT('',(-5.5,-7.5,4.));
#2250=CARTESIAN_POINT('',(-5.75,-7.5,3.75));
#2251=CARTESIAN_POINT('Origin',(-8.,-7.5,4.));
#2252=CARTESIAN_POINT('Origin',(0.,0.,4.));
#2253=CARTESIAN_POINT('',(-11.,8.,4.));
#2254=CARTESIAN_POINT('',(-11.,-11.,4.));
#2255=CARTESIAN_POINT('',(-11.,-5.,4.));
#2256=CARTESIAN_POINT('',(11.,-11.,4.));
#2257=CARTESIAN_POINT('',(-11.,-11.,4.));
#2258=CARTESIAN_POINT('',(11.,11.,4.));
#2259=CARTESIAN_POINT('',(11.,-11.,4.));
#2260=CARTESIAN_POINT('',(-8.,11.,4.));
#2261=CARTESIAN_POINT('',(11.,11.,4.));
#2262=CARTESIAN_POINT('',(-11.,8.,4.));
#2263=CARTESIAN_POINT('',(10.5,-7.5,4.));
#2264=CARTESIAN_POINT('Origin',(8.,-7.5,4.));
#2265=CARTESIAN_POINT('',(-8.,3.,4.));
#2266=CARTESIAN_POINT('Origin',(-3.,3.,4.));
#2267=CARTESIAN_POINT('',(10.5,7.5,4.));
#2268=CARTESIAN_POINT('Origin',(8.,7.5,4.));
#2269=CARTESIAN_POINT('Origin',(-8.,-7.5,4.));
#2270=CARTESIAN_POINT('',(-6.,-7.5,3.));
#2271=CARTESIAN_POINT('',(-6.,-7.5,4.));
#2272=CARTESIAN_POINT('Origin',(-8.,-7.5,3.));
#2273=CARTESIAN_POINT('Origin',(8.,-7.5,3.75));
#2274=CARTESIAN_POINT('',(10.,-7.5,3.5));
#2275=CARTESIAN_POINT('Origin',(8.,-7.5,3.5));
#2276=CARTESIAN_POINT('',(10.25,-7.5,3.75));
#2277=CARTESIAN_POINT('Origin',(8.,-7.5,4.));
#2278=CARTESIAN_POINT('',(10.,-7.5,3.));
#2279=CARTESIAN_POINT('',(10.,-7.5,4.));
#2280=CARTESIAN_POINT('Origin',(8.,-7.5,3.));
#2281=CARTESIAN_POINT('Origin',(8.,7.5,3.75));
#2282=CARTESIAN_POINT('',(10.,7.5,3.5));
#2283=CARTESIAN_POINT('Origin',(8.,7.5,3.5));
#2284=CARTESIAN_POINT('',(10.25,7.5,3.75));
#2285=CARTESIAN_POINT('Origin',(8.,7.5,4.));
#2286=CARTESIAN_POINT('',(10.,7.5,3.));
#2287=CARTESIAN_POINT('',(10.,7.5,4.));
#2288=CARTESIAN_POINT('Origin',(8.,7.5,3.));
#2289=CARTESIAN_POINT('Origin',(8.,7.5,3.));
#2290=CARTESIAN_POINT('Origin',(8.,-7.5,3.));
#2291=CARTESIAN_POINT('Origin',(-8.,-7.5,3.));
#2292=CARTESIAN_POINT('Origin',(-3.,3.,0.));
#2293=CARTESIAN_POINT('',(-8.,3.,0.));
#2294=CARTESIAN_POINT('Origin',(-3.,3.,0.));
#2295=CARTESIAN_POINT('',(-8.,3.,0.));
#2296=CARTESIAN_POINT('Origin',(-8.,11.,0.));
#2297=CARTESIAN_POINT('',(-11.,8.,0.));
#2298=CARTESIAN_POINT('',(-8.,11.,0.));
#2299=CARTESIAN_POINT('',(-11.,8.,0.));
#2300=CARTESIAN_POINT('',(-11.,8.,0.));
#2301=CARTESIAN_POINT('',(-8.,11.,0.));
#2302=CARTESIAN_POINT('Origin',(11.,11.,0.));
#2303=CARTESIAN_POINT('',(11.,11.,0.));
#2304=CARTESIAN_POINT('',(11.,11.,0.));
#2305=CARTESIAN_POINT('',(11.,11.,0.));
#2306=CARTESIAN_POINT('Origin',(11.,-11.,0.));
#2307=CARTESIAN_POINT('',(11.,-11.,0.));
#2308=CARTESIAN_POINT('',(11.,-11.,0.));
#2309=CARTESIAN_POINT('',(11.,-11.,0.));
#2310=CARTESIAN_POINT('Origin',(-11.,-11.,0.));
#2311=CARTESIAN_POINT('',(-11.,-11.,0.));
#2312=CARTESIAN_POINT('',(-11.,-11.,0.));
#2313=CARTESIAN_POINT('',(-11.,-11.,0.));
#2314=CARTESIAN_POINT('Origin',(-11.,8.,0.));
#2315=CARTESIAN_POINT('',(-11.,-5.,0.));
#2316=CARTESIAN_POINT('Origin',(0.,0.,0.));
#2317=CARTESIAN_POINT('',(0.,0.,0.));
#2318=CARTESIAN_POINT('Origin',(8.,-7.5,10.5));
#2319=CARTESIAN_POINT('',(10.,-7.5,10.5));
#2320=CARTESIAN_POINT('Origin',(8.,-7.5,10.5));
#2321=CARTESIAN_POINT('',(9.,-7.5,10.5));
#2322=CARTESIAN_POINT('Origin',(8.,-7.5,10.5));
#2323=CARTESIAN_POINT('Origin',(8.,-7.5,12.5));
#2324=CARTESIAN_POINT('',(9.,-7.5,12.3));
#2325=CARTESIAN_POINT('Origin',(8.,-7.5,12.3));
#2326=CARTESIAN_POINT('',(9.,-7.5,12.5));
#2327=CARTESIAN_POINT('Origin',(8.,-7.5,12.4));
#2328=CARTESIAN_POINT('',(9.2,-7.5,12.5));
#2329=CARTESIAN_POINT('',(9.1,-7.5,12.4));
#2330=CARTESIAN_POINT('Origin',(8.,-7.5,12.5));
#2331=CARTESIAN_POINT('Origin',(8.,-7.5,12.5));
#2332=CARTESIAN_POINT('',(10.,-7.5,12.3));
#2333=CARTESIAN_POINT('',(10.,-7.5,12.5));
#2334=CARTESIAN_POINT('Origin',(8.,-7.5,12.3));
#2335=CARTESIAN_POINT('Origin',(8.,-7.5,12.5));
#2336=CARTESIAN_POINT('',(9.8,-7.5,12.5));
#2337=CARTESIAN_POINT('Origin',(8.,-7.5,12.5));
#2338=CARTESIAN_POINT('Origin',(8.,-7.5,12.4));
#2339=CARTESIAN_POINT('',(9.9,-7.5,12.4));
#2340=CARTESIAN_POINT('Origin',(8.,-7.5,4.5));
#2341=CARTESIAN_POINT('',(9.,-7.5,4.5));
#2342=CARTESIAN_POINT('Origin',(8.,-7.5,4.5));
#2343=CARTESIAN_POINT('',(7.13397459621556,-7.5,4.5));
#2344=CARTESIAN_POINT('Origin',(8.,-7.5,4.5));
#2345=CARTESIAN_POINT('Origin',(8.,-7.5,12.5));
#2346=CARTESIAN_POINT('',(9.,-7.5,6.7));
#2347=CARTESIAN_POINT('',(9.,-7.5,12.5));
#2348=CARTESIAN_POINT('Origin',(8.,-7.5,6.7));
#2349=CARTESIAN_POINT('Origin',(8.,-7.5,10.5));
#2350=CARTESIAN_POINT('',(9.,-7.5,10.5));
#2351=CARTESIAN_POINT('Origin',(8.,-7.5,10.5));
#2352=CARTESIAN_POINT('Origin',(8.,-7.5,12.5));
#2353=CARTESIAN_POINT('',(9.,-7.5,7.5));
#2354=CARTESIAN_POINT('Origin',(8.,-7.5,7.5));
#2355=CARTESIAN_POINT('',(9.,-7.5,12.5));
#2356=CARTESIAN_POINT('Origin',(8.,-7.5,7.5));
#2357=CARTESIAN_POINT('',(10.,-7.5,7.5));
#2358=CARTESIAN_POINT('Origin',(8.,-7.5,7.5));
#2359=CARTESIAN_POINT('Origin',(8.,-7.5,12.5));
#2360=CARTESIAN_POINT('',(10.,-7.5,6.7));
#2361=CARTESIAN_POINT('Origin',(8.,-7.5,6.7));
#2362=CARTESIAN_POINT('',(10.,-7.5,12.5));
#2363=CARTESIAN_POINT('Origin',(8.,-7.5,6.6));
#2364=CARTESIAN_POINT('',(9.8,-7.5,6.5));
#2365=CARTESIAN_POINT('',(9.9,-7.5,6.6));
#2366=CARTESIAN_POINT('Origin',(8.,-7.5,6.5));
#2367=CARTESIAN_POINT('Origin',(8.,-7.5,6.5));
#2368=CARTESIAN_POINT('',(9.2,-7.5,6.5));
#2369=CARTESIAN_POINT('Origin',(8.,-7.5,6.5));
#2370=CARTESIAN_POINT('Origin',(8.,-7.5,6.6));
#2371=CARTESIAN_POINT('',(9.1,-7.5,6.6));
#2372=CARTESIAN_POINT('Origin',(8.,-7.5,4.));
#2373=CARTESIAN_POINT('',(8.,-7.5,5.));
#2374=CARTESIAN_POINT('Origin',(8.,-7.5,4.));
#2375=CARTESIAN_POINT('',(0.,0.,0.));
#2376=CARTESIAN_POINT('Origin',(8.,7.5,10.5));
#2377=CARTESIAN_POINT('',(10.,7.5,10.5));
#2378=CARTESIAN_POINT('Origin',(8.,7.5,10.5));
#2379=CARTESIAN_POINT('',(9.,7.5,10.5));
#2380=CARTESIAN_POINT('Origin',(8.,7.5,10.5));
#2381=CARTESIAN_POINT('Origin',(8.,7.5,12.5));
#2382=CARTESIAN_POINT('',(9.,7.5,12.3));
#2383=CARTESIAN_POINT('Origin',(8.,7.5,12.3));
#2384=CARTESIAN_POINT('',(9.,7.5,12.5));
#2385=CARTESIAN_POINT('Origin',(8.,7.5,12.4));
#2386=CARTESIAN_POINT('',(9.2,7.5,12.5));
#2387=CARTESIAN_POINT('',(9.1,7.5,12.4));
#2388=CARTESIAN_POINT('Origin',(8.,7.5,12.5));
#2389=CARTESIAN_POINT('Origin',(8.,7.5,12.5));
#2390=CARTESIAN_POINT('',(10.,7.5,12.3));
#2391=CARTESIAN_POINT('',(10.,7.5,12.5));
#2392=CARTESIAN_POINT('Origin',(8.,7.5,12.3));
#2393=CARTESIAN_POINT('Origin',(8.,7.5,12.5));
#2394=CARTESIAN_POINT('',(9.8,7.5,12.5));
#2395=CARTESIAN_POINT('Origin',(8.,7.5,12.5));
#2396=CARTESIAN_POINT('Origin',(8.,7.5,12.4));
#2397=CARTESIAN_POINT('',(9.9,7.5,12.4));
#2398=CARTESIAN_POINT('Origin',(8.,7.5,4.5));
#2399=CARTESIAN_POINT('',(9.,7.5,4.5));
#2400=CARTESIAN_POINT('Origin',(8.,7.5,4.5));
#2401=CARTESIAN_POINT('',(7.13397459621556,7.5,4.5));
#2402=CARTESIAN_POINT('Origin',(8.,7.5,4.5));
#2403=CARTESIAN_POINT('Origin',(8.,7.5,12.5));
#2404=CARTESIAN_POINT('',(9.,7.5,6.7));
#2405=CARTESIAN_POINT('',(9.,7.5,12.5));
#2406=CARTESIAN_POINT('Origin',(8.,7.5,6.7));
#2407=CARTESIAN_POINT('Origin',(8.,7.5,10.5));
#2408=CARTESIAN_POINT('',(9.,7.5,10.5));
#2409=CARTESIAN_POINT('Origin',(8.,7.5,10.5));
#2410=CARTESIAN_POINT('Origin',(8.,7.5,12.5));
#2411=CARTESIAN_POINT('',(9.,7.5,7.5));
#2412=CARTESIAN_POINT('Origin',(8.,7.5,7.5));
#2413=CARTESIAN_POINT('',(9.,7.5,12.5));
#2414=CARTESIAN_POINT('Origin',(8.,7.5,7.5));
#2415=CARTESIAN_POINT('',(10.,7.5,7.5));
#2416=CARTESIAN_POINT('Origin',(8.,7.5,7.5));
#2417=CARTESIAN_POINT('Origin',(8.,7.5,12.5));
#2418=CARTESIAN_POINT('',(10.,7.5,6.7));
#2419=CARTESIAN_POINT('Origin',(8.,7.5,6.7));
#2420=CARTESIAN_POINT('',(10.,7.5,12.5));
#2421=CARTESIAN_POINT('Origin',(8.,7.5,6.6));
#2422=CARTESIAN_POINT('',(9.8,7.5,6.5));
#2423=CARTESIAN_POINT('',(9.9,7.5,6.6));
#2424=CARTESIAN_POINT('Origin',(8.,7.5,6.5));
#2425=CARTESIAN_POINT('Origin',(8.,7.5,6.5));
#2426=CARTESIAN_POINT('',(9.2,7.5,6.5));
#2427=CARTESIAN_POINT('Origin',(8.,7.5,6.5));
#2428=CARTESIAN_POINT('Origin',(8.,7.5,6.6));
#2429=CARTESIAN_POINT('',(9.1,7.5,6.6));
#2430=CARTESIAN_POINT('Origin',(8.,7.5,4.));
#2431=CARTESIAN_POINT('',(8.,7.5,5.));
#2432=CARTESIAN_POINT('Origin',(8.,7.5,4.));
#2433=CARTESIAN_POINT('',(0.,0.,0.));
#2434=CARTESIAN_POINT('Origin',(-8.,-7.5,10.5));
#2435=CARTESIAN_POINT('',(-6.,-7.5,10.5));
#2436=CARTESIAN_POINT('Origin',(-8.,-7.5,10.5));
#2437=CARTESIAN_POINT('',(-7.,-7.5,10.5));
#2438=CARTESIAN_POINT('Origin',(-8.,-7.5,10.5));
#2439=CARTESIAN_POINT('Origin',(-8.,-7.5,12.5));
#2440=CARTESIAN_POINT('',(-7.,-7.5,12.3));
#2441=CARTESIAN_POINT('Origin',(-8.,-7.5,12.3));
#2442=CARTESIAN_POINT('',(-7.,-7.5,12.5));
#2443=CARTESIAN_POINT('Origin',(-8.,-7.5,12.4));
#2444=CARTESIAN_POINT('',(-6.8,-7.5,12.5));
#2445=CARTESIAN_POINT('',(-6.9,-7.5,12.4));
#2446=CARTESIAN_POINT('Origin',(-8.,-7.5,12.5));
#2447=CARTESIAN_POINT('Origin',(-8.,-7.5,12.5));
#2448=CARTESIAN_POINT('',(-6.,-7.5,12.3));
#2449=CARTESIAN_POINT('',(-6.,-7.5,12.5));
#2450=CARTESIAN_POINT('Origin',(-8.,-7.5,12.3));
#2451=CARTESIAN_POINT('Origin',(-8.,-7.5,12.5));
#2452=CARTESIAN_POINT('',(-6.2,-7.5,12.5));
#2453=CARTESIAN_POINT('Origin',(-8.,-7.5,12.5));
#2454=CARTESIAN_POINT('Origin',(-8.,-7.5,12.4));
#2455=CARTESIAN_POINT('',(-6.1,-7.5,12.4));
#2456=CARTESIAN_POINT('Origin',(-8.,-7.5,4.5));
#2457=CARTESIAN_POINT('',(-7.,-7.5,4.5));
#2458=CARTESIAN_POINT('Origin',(-8.,-7.5,4.5));
#2459=CARTESIAN_POINT('',(-8.86602540378444,-7.5,4.5));
#2460=CARTESIAN_POINT('Origin',(-8.,-7.5,4.5));
#2461=CARTESIAN_POINT('Origin',(-8.,-7.5,12.5));
#2462=CARTESIAN_POINT('',(-7.,-7.5,6.7));
#2463=CARTESIAN_POINT('',(-7.,-7.5,12.5));
#2464=CARTESIAN_POINT('Origin',(-8.,-7.5,6.7));
#2465=CARTESIAN_POINT('Origin',(-8.,-7.5,10.5));
#2466=CARTESIAN_POINT('',(-7.,-7.5,10.5));
#2467=CARTESIAN_POINT('Origin',(-8.,-7.5,10.5));
#2468=CARTESIAN_POINT('Origin',(-8.,-7.5,12.5));
#2469=CARTESIAN_POINT('',(-7.,-7.5,7.5));
#2470=CARTESIAN_POINT('Origin',(-8.,-7.5,7.5));
#2471=CARTESIAN_POINT('',(-7.,-7.5,12.5));
#2472=CARTESIAN_POINT('Origin',(-8.,-7.5,7.5));
#2473=CARTESIAN_POINT('',(-6.,-7.5,7.5));
#2474=CARTESIAN_POINT('Origin',(-8.,-7.5,7.5));
#2475=CARTESIAN_POINT('Origin',(-8.,-7.5,12.5));
#2476=CARTESIAN_POINT('',(-6.,-7.5,6.7));
#2477=CARTESIAN_POINT('Origin',(-8.,-7.5,6.7));
#2478=CARTESIAN_POINT('',(-6.,-7.5,12.5));
#2479=CARTESIAN_POINT('Origin',(-8.,-7.5,6.6));
#2480=CARTESIAN_POINT('',(-6.2,-7.5,6.5));
#2481=CARTESIAN_POINT('',(-6.1,-7.5,6.6));
#2482=CARTESIAN_POINT('Origin',(-8.,-7.5,6.5));
#2483=CARTESIAN_POINT('Origin',(-8.,-7.5,6.5));
#2484=CARTESIAN_POINT('',(-6.8,-7.5,6.5));
#2485=CARTESIAN_POINT('Origin',(-8.,-7.5,6.5));
#2486=CARTESIAN_POINT('Origin',(-8.,-7.5,6.6));
#2487=CARTESIAN_POINT('',(-6.9,-7.5,6.6));
#2488=CARTESIAN_POINT('Origin',(-8.,-7.5,4.));
#2489=CARTESIAN_POINT('',(-8.,-7.5,5.));
#2490=CARTESIAN_POINT('Origin',(-8.,-7.5,4.));
#2491=CARTESIAN_POINT('',(0.,0.,0.));
#2492=CARTESIAN_POINT('Origin',(8.,7.5,4.));
#2493=CARTESIAN_POINT('',(8.,7.5,5.));
#2494=CARTESIAN_POINT('',(8.,7.5,3.));
#2495=CARTESIAN_POINT('Origin',(8.,7.5,4.));
#2496=CARTESIAN_POINT('',(0.,0.,0.));
#2497=CARTESIAN_POINT('Origin',(8.,-7.5,4.));
#2498=CARTESIAN_POINT('',(8.,-7.5,5.));
#2499=CARTESIAN_POINT('',(8.,-7.5,3.));
#2500=CARTESIAN_POINT('Origin',(8.,-7.5,4.));
#2501=CARTESIAN_POINT('',(0.,0.,0.));
#2502=CARTESIAN_POINT('Origin',(-8.,-7.5,4.));
#2503=CARTESIAN_POINT('',(-8.,-7.5,5.));
#2504=CARTESIAN_POINT('',(-8.,-7.5,3.));
#2505=CARTESIAN_POINT('Origin',(-8.,-7.5,4.));
#2506=CARTESIAN_POINT('',(0.,0.,0.));
#2507=CARTESIAN_POINT('Origin',(-8.,-7.5,12.35));
#2508=CARTESIAN_POINT('',(-6.,-7.5,12.2));
#2509=CARTESIAN_POINT('Origin',(-8.,-7.5,12.2));
#2510=CARTESIAN_POINT('',(-5.7,-7.5,12.5));
#2511=CARTESIAN_POINT('',(-5.85,-7.5,12.35));
#2512=CARTESIAN_POINT('Origin',(-8.,-7.5,12.5));
#2513=CARTESIAN_POINT('Origin',(0.,0.,12.5));
#2514=CARTESIAN_POINT('',(-9.79289321881345,-10.,12.5));
#2515=CARTESIAN_POINT('',(-10.5,-9.29289321881345,12.5));
#2516=CARTESIAN_POINT('',(-10.0214466094067,-9.77144660940673,12.5));
#2517=CARTESIAN_POINT('',(9.79289321881345,-10.,12.5));
#2518=CARTESIAN_POINT('',(-5.5,-10.,12.5));
#2519=CARTESIAN_POINT('',(10.5,-9.29289321881345,12.5));
#2520=CARTESIAN_POINT('',(10.0214466094067,-9.77144660940673,12.5));
#2521=CARTESIAN_POINT('',(10.5,9.79289321881345,12.5));
#2522=CARTESIAN_POINT('',(10.5,-5.5,12.5));
#2523=CARTESIAN_POINT('',(9.79289321881345,10.5,12.5));
#2524=CARTESIAN_POINT('',(10.1464466094067,10.1464466094067,12.5));
#2525=CARTESIAN_POINT('',(6.20710678118655,10.5,12.5));
#2526=CARTESIAN_POINT('',(5.5,10.5,12.5));
#2527=CARTESIAN_POINT('',(5.5,9.79289321881345,12.5));
#2528=CARTESIAN_POINT('',(1.85355339059327,6.14644660940672,12.5));
#2529=CARTESIAN_POINT('',(5.5,-5.,12.5));
#2530=CARTESIAN_POINT('',(5.5,5.5,12.5));
#2531=CARTESIAN_POINT('',(-9.79289321881345,-5.,12.5));
#2532=CARTESIAN_POINT('',(2.5,-5.,12.5));
#2533=CARTESIAN_POINT('',(-10.5,-5.70710678118654,12.5));
#2534=CARTESIAN_POINT('',(-6.27144660940672,-1.47855339059328,12.5));
#2535=CARTESIAN_POINT('',(-10.5,-2.5,12.5));
#2536=CARTESIAN_POINT('',(10.3,-7.5,12.5));
#2537=CARTESIAN_POINT('Origin',(8.,-7.5,12.5));
#2538=CARTESIAN_POINT('',(10.3,7.5,12.5));
#2539=CARTESIAN_POINT('Origin',(8.,7.5,12.5));
#2540=CARTESIAN_POINT('Origin',(-8.,-7.5,12.5));
#2541=CARTESIAN_POINT('',(-6.,-7.5,7.5));
#2542=CARTESIAN_POINT('',(-6.,-7.5,12.5));
#2543=CARTESIAN_POINT('Origin',(-8.,-7.5,7.5));
#2544=CARTESIAN_POINT('Origin',(8.,-7.5,12.35));
#2545=CARTESIAN_POINT('',(10.,-7.5,12.2));
#2546=CARTESIAN_POINT('Origin',(8.,-7.5,12.2));
#2547=CARTESIAN_POINT('',(10.15,-7.5,12.35));
#2548=CARTESIAN_POINT('Origin',(8.,-7.5,12.5));
#2549=CARTESIAN_POINT('',(10.,-7.5,7.5));
#2550=CARTESIAN_POINT('',(10.,-7.5,12.5));
#2551=CARTESIAN_POINT('Origin',(8.,-7.5,7.5));
#2552=CARTESIAN_POINT('Origin',(-10.1982233047034,-9.94822330470336,12.25));
#2553=CARTESIAN_POINT('',(-11.,-9.5,12.));
#2554=CARTESIAN_POINT('',(-10.,-10.5,12.));
#2555=CARTESIAN_POINT('',(-10.375,-10.125,12.));
#2556=CARTESIAN_POINT('',(-9.7059086127755,-9.7900005843855,12.7099994156145));
#2557=CARTESIAN_POINT('',(-10.5,-9.29289321881345,12.5));
#2558=CARTESIAN_POINT('Origin',(-10.75,-2.5,12.25));
#2559=CARTESIAN_POINT('',(-11.,-5.5,12.));
#2560=CARTESIAN_POINT('',(-10.5,-5.70710678118654,12.5));
#2561=CARTESIAN_POINT('',(-11.,-2.5,12.));
#2562=CARTESIAN_POINT('Origin',(-6.44822330470336,-1.30177669529664,12.25));
#2563=CARTESIAN_POINT('',(-10.,-4.5,12.));
#2564=CARTESIAN_POINT('',(-9.79289321881345,-5.,12.5));
#2565=CARTESIAN_POINT('',(-6.62499999999999,-1.125,12.));
#2566=CARTESIAN_POINT('Origin',(2.5,-4.75,12.25));
#2567=CARTESIAN_POINT('',(5.,-4.5,12.));
#2568=CARTESIAN_POINT('',(3.08333333333333,-2.58333333333333,10.0833333333333));
#2569=CARTESIAN_POINT('',(2.5,-4.5,12.));
#2570=CARTESIAN_POINT('Origin',(-10.5,-10.,7.5));
#2571=CARTESIAN_POINT('',(-11.,-9.5,7.5));
#2572=CARTESIAN_POINT('',(-11.,-9.5,7.5));
#2573=CARTESIAN_POINT('',(-10.,-10.5,7.5));
#2574=CARTESIAN_POINT('',(-10.375,-10.125,7.5));
#2575=CARTESIAN_POINT('',(-10.,-10.5,7.5));
#2576=CARTESIAN_POINT('Origin',(-11.,-5.,7.5));
#2577=CARTESIAN_POINT('',(-11.,-5.5,7.5));
#2578=CARTESIAN_POINT('',(-11.,-5.5,7.5));
#2579=CARTESIAN_POINT('',(-11.,8.,7.5));
#2580=CARTESIAN_POINT('Origin',(-10.5,-5.,7.5));
#2581=CARTESIAN_POINT('',(-10.,-4.5,7.5));
#2582=CARTESIAN_POINT('',(-10.,-4.5,7.5));
#2583=CARTESIAN_POINT('',(-6.62499999999999,-1.125,7.5));
#2584=CARTESIAN_POINT('Origin',(5.,-4.5,7.5));
#2585=CARTESIAN_POINT('',(5.,-4.5,7.5));
#2586=CARTESIAN_POINT('',(5.,-4.5,7.5));
#2587=CARTESIAN_POINT('',(2.5,-4.5,7.5));
#2588=CARTESIAN_POINT('Origin',(0.,0.,7.5));
#2589=CARTESIAN_POINT('',(5.,10.,7.5));
#2590=CARTESIAN_POINT('',(5.,11.,7.5));
#2591=CARTESIAN_POINT('',(6.,11.,7.5));
#2592=CARTESIAN_POINT('',(1.5,6.5,7.5));
#2593=CARTESIAN_POINT('',(10.,11.,7.5));
#2594=CARTESIAN_POINT('',(5.,11.,7.5));
#2595=CARTESIAN_POINT('',(11.,10.,7.5));
#2596=CARTESIAN_POINT('',(10.5,10.5,7.5));
#2597=CARTESIAN_POINT('',(11.,-9.5,7.5));
#2598=CARTESIAN_POINT('',(11.,-11.,7.5));
#2599=CARTESIAN_POINT('',(10.,-10.5,7.5));
#2600=CARTESIAN_POINT('',(10.375,-10.125,7.5));
#2601=CARTESIAN_POINT('',(-5.5,-10.5,7.5));
#2602=CARTESIAN_POINT('',(10.,7.5,7.5));
#2603=CARTESIAN_POINT('Origin',(8.,7.5,7.5));
#2604=CARTESIAN_POINT('Origin',(5.25,5.5,12.25));
#2605=CARTESIAN_POINT('',(5.,10.,12.));
#2606=CARTESIAN_POINT('',(5.,5.5,12.));
#2607=CARTESIAN_POINT('',(5.5,9.79289321881345,12.5));
#2608=CARTESIAN_POINT('Origin',(5.5,10.75,12.25));
#2609=CARTESIAN_POINT('',(10.,11.,12.));
#2610=CARTESIAN_POINT('',(9.79289321881345,10.5,12.5));
#2611=CARTESIAN_POINT('',(6.,11.,12.));
#2612=CARTESIAN_POINT('',(5.5,11.,12.));
#2613=CARTESIAN_POINT('',(6.,11.,12.));
#2614=CARTESIAN_POINT('Origin',(10.3232233047034,10.3232233047034,12.25));
#2615=CARTESIAN_POINT('',(11.,10.,12.));
#2616=CARTESIAN_POINT('',(10.5,9.79289321881345,12.5));
#2617=CARTESIAN_POINT('',(10.5,10.5,12.));
#2618=CARTESIAN_POINT('Origin',(10.75,-5.5,12.25));
#2619=CARTESIAN_POINT('',(11.,-9.5,12.));
#2620=CARTESIAN_POINT('',(10.5,-9.29289321881345,12.5));
#2621=CARTESIAN_POINT('',(11.,-5.5,12.));
#2622=CARTESIAN_POINT('Origin',(10.1982233047034,-9.94822330470337,12.25));
#2623=CARTESIAN_POINT('',(10.,-10.5,12.));
#2624=CARTESIAN_POINT('',(9.79289321881345,-10.,12.5));
#2625=CARTESIAN_POINT('',(10.375,-10.125,12.));
#2626=CARTESIAN_POINT('Origin',(-5.5,-10.25,12.25));
#2627=CARTESIAN_POINT('',(-5.5,-10.5,12.));
#2628=CARTESIAN_POINT('Origin',(1.67677669529664,6.32322330470336,12.25));
#2629=CARTESIAN_POINT('',(1.5,6.5,12.));
#2630=CARTESIAN_POINT('Origin',(5.,11.,7.5));
#2631=CARTESIAN_POINT('',(5.,10.,7.5));
#2632=CARTESIAN_POINT('Origin',(5.5,10.5,7.5));
#2633=CARTESIAN_POINT('',(6.,11.,7.5));
#2634=CARTESIAN_POINT('Origin',(11.,11.,7.5));
#2635=CARTESIAN_POINT('',(10.,11.,7.5));
#2636=CARTESIAN_POINT('Origin',(10.5,10.5,7.5));
#2637=CARTESIAN_POINT('',(11.,10.,7.5));
#2638=CARTESIAN_POINT('Origin',(11.,-11.,7.5));
#2639=CARTESIAN_POINT('',(11.,-9.5,7.5));
#2640=CARTESIAN_POINT('Origin',(10.5,-10.,7.5));
#2641=CARTESIAN_POINT('',(10.,-10.5,7.5));
#2642=CARTESIAN_POINT('Origin',(-11.,-10.5,7.5));
#2643=CARTESIAN_POINT('Origin',(8.,7.5,12.35));
#2644=CARTESIAN_POINT('',(10.,7.5,12.2));
#2645=CARTESIAN_POINT('Origin',(8.,7.5,12.2));
#2646=CARTESIAN_POINT('',(10.15,7.5,12.35));
#2647=CARTESIAN_POINT('Origin',(8.,7.5,12.5));
#2648=CARTESIAN_POINT('',(10.,7.5,12.5));
#2649=CARTESIAN_POINT('',(0.,0.,0.));
#2650=CARTESIAN_POINT('',(0.,0.,0.));
#2651=CARTESIAN_POINT('',(0.,0.,0.));
#2652=CARTESIAN_POINT('',(0.,0.,0.));
#2653=CARTESIAN_POINT('',(0.,0.,0.));
#2654=CARTESIAN_POINT('',(0.,0.,0.));
#2655=CARTESIAN_POINT('',(0.,0.,0.));
#2656=CARTESIAN_POINT('',(0.,0.,0.));
#2657=UNCERTAINTY_MEASURE_WITH_UNIT(LENGTH_MEASURE(0.01),#2677,
'DISTANCE_ACCURACY_VALUE',
'Maximum model space distance between geometric entities at asserted c
onnectivities');
#2658=UNCERTAINTY_MEASURE_WITH_UNIT(LENGTH_MEASURE(0.01),#2677,
'DISTANCE_ACCURACY_VALUE',
'Maximum model space distance between geometric entities at asserted c
onnectivities');
#2659=UNCERTAINTY_MEASURE_WITH_UNIT(LENGTH_MEASURE(0.01),#2677,
'DISTANCE_ACCURACY_VALUE',
'Maximum model space distance between geometric entities at asserted c
onnectivities');
#2660=UNCERTAINTY_MEASURE_WITH_UNIT(LENGTH_MEASURE(0.01),#2677,
'DISTANCE_ACCURACY_VALUE',
'Maximum model space distance between geometric entities at asserted c
onnectivities');
#2661=UNCERTAINTY_MEASURE_WITH_UNIT(LENGTH_MEASURE(0.01),#2677,
'DISTANCE_ACCURACY_VALUE',
'Maximum model space distance between geometric entities at asserted c
onnectivities');
#2662=UNCERTAINTY_MEASURE_WITH_UNIT(LENGTH_MEASURE(0.01),#2677,
'DISTANCE_ACCURACY_VALUE',
'Maximum model space distance between geometric entities at asserted c
onnectivities');
#2663=UNCERTAINTY_MEASURE_WITH_UNIT(LENGTH_MEASURE(0.01),#2677,
'DISTANCE_ACCURACY_VALUE',
'Maximum model space distance between geometric entities at asserted c
onnectivities');
#2664=UNCERTAINTY_MEASURE_WITH_UNIT(LENGTH_MEASURE(0.01),#2677,
'DISTANCE_ACCURACY_VALUE',
'Maximum model space distance between geometric entities at asserted c
onnectivities');
#2665=UNCERTAINTY_MEASURE_WITH_UNIT(LENGTH_MEASURE(0.01),#2677,
'DISTANCE_ACCURACY_VALUE',
'Maximum model space distance between geometric entities at asserted c
onnectivities');
#2666=UNCERTAINTY_MEASURE_WITH_UNIT(LENGTH_MEASURE(0.01),#2677,
'DISTANCE_ACCURACY_VALUE',
'Maximum model space distance between geometric entities at asserted c
onnectivities');
#2667=(
GEOMETRIC_REPRESENTATION_CONTEXT(3)
GLOBAL_UNCERTAINTY_ASSIGNED_CONTEXT((#2657))
GLOBAL_UNIT_ASSIGNED_CONTEXT((#2677,#2679,#2680))
REPRESENTATION_CONTEXT('','3D')
);
#2668=(
GEOMETRIC_REPRESENTATION_CONTEXT(3)
GLOBAL_UNCERTAINTY_ASSIGNED_CONTEXT((#2658))
GLOBAL_UNIT_ASSIGNED_CONTEXT((#2677,#2679,#2680))
REPRESENTATION_CONTEXT('','3D')
);
#2669=(
GEOMETRIC_REPRESENTATION_CONTEXT(3)
GLOBAL_UNCERTAINTY_ASSIGNED_CONTEXT((#2659))
GLOBAL_UNIT_ASSIGNED_CONTEXT((#2677,#2679,#2680))
REPRESENTATION_CONTEXT('','3D')
);
#2670=(
GEOMETRIC_REPRESENTATION_CONTEXT(3)
GLOBAL_UNCERTAINTY_ASSIGNED_CONTEXT((#2660))
GLOBAL_UNIT_ASSIGNED_CONTEXT((#2677,#2679,#2680))
REPRESENTATION_CONTEXT('','3D')
);
#2671=(
GEOMETRIC_REPRESENTATION_CONTEXT(3)
GLOBAL_UNCERTAINTY_ASSIGNED_CONTEXT((#2661))
GLOBAL_UNIT_ASSIGNED_CONTEXT((#2677,#2679,#2680))
REPRESENTATION_CONTEXT('','3D')
);
#2672=(
GEOMETRIC_REPRESENTATION_CONTEXT(3)
GLOBAL_UNCERTAINTY_ASSIGNED_CONTEXT((#2662))
GLOBAL_UNIT_ASSIGNED_CONTEXT((#2677,#2679,#2680))
REPRESENTATION_CONTEXT('','3D')
);
#2673=(
GEOMETRIC_REPRESENTATION_CONTEXT(3)
GLOBAL_UNCERTAINTY_ASSIGNED_CONTEXT((#2663))
GLOBAL_UNIT_ASSIGNED_CONTEXT((#2677,#2679,#2680))
REPRESENTATION_CONTEXT('','3D')
);
#2674=(
GEOMETRIC_REPRESENTATION_CONTEXT(3)
GLOBAL_UNCERTAINTY_ASSIGNED_CONTEXT((#2664))
GLOBAL_UNIT_ASSIGNED_CONTEXT((#2677,#2679,#2680))
REPRESENTATION_CONTEXT('','3D')
);
#2675=(
GEOMETRIC_REPRESENTATION_CONTEXT(3)
GLOBAL_UNCERTAINTY_ASSIGNED_CONTEXT((#2665))
GLOBAL_UNIT_ASSIGNED_CONTEXT((#2677,#2679,#2680))
REPRESENTATION_CONTEXT('','3D')
);
#2676=(
GEOMETRIC_REPRESENTATION_CONTEXT(3)
GLOBAL_UNCERTAINTY_ASSIGNED_CONTEXT((#2666))
GLOBAL_UNIT_ASSIGNED_CONTEXT((#2677,#2679,#2680))
REPRESENTATION_CONTEXT('','3D')
);
#2677=(
LENGTH_UNIT()
NAMED_UNIT(*)
SI_UNIT(.MILLI.,.METRE.)
);
#2678=(
LENGTH_UNIT()
NAMED_UNIT(*)
SI_UNIT($,.METRE.)
);
#2679=(
NAMED_UNIT(*)
PLANE_ANGLE_UNIT()
SI_UNIT($,.RADIAN.)
);
#2680=(
NAMED_UNIT(*)
SI_UNIT($,.STERADIAN.)
SOLID_ANGLE_UNIT()
);
#2681=SHAPE_DEFINITION_REPRESENTATION(#2690,#2707);
#2682=SHAPE_DEFINITION_REPRESENTATION(#2691,#2708);
#2683=SHAPE_DEFINITION_REPRESENTATION(#2692,#2709);
#2684=SHAPE_DEFINITION_REPRESENTATION(#2693,#2710);
#2685=SHAPE_DEFINITION_REPRESENTATION(#2694,#2711);
#2686=SHAPE_DEFINITION_REPRESENTATION(#2695,#2712);
#2687=SHAPE_DEFINITION_REPRESENTATION(#2696,#2713);
#2688=SHAPE_DEFINITION_REPRESENTATION(#2697,#2714);
#2689=SHAPE_DEFINITION_REPRESENTATION(#2698,#2715);
#2690=PRODUCT_DEFINITION_SHAPE('',$,#2717);
#2691=PRODUCT_DEFINITION_SHAPE('',$,#2718);
#2692=PRODUCT_DEFINITION_SHAPE('',$,#2719);
#2693=PRODUCT_DEFINITION_SHAPE('',$,#2720);
#2694=PRODUCT_DEFINITION_SHAPE('',$,#2721);
#2695=PRODUCT_DEFINITION_SHAPE('',$,#2722);
#2696=PRODUCT_DEFINITION_SHAPE('',$,#2723);
#2697=PRODUCT_DEFINITION_SHAPE('',$,#2724);
#2698=PRODUCT_DEFINITION_SHAPE('',$,#2725);
#2699=PRODUCT_DEFINITION_SHAPE($,$,#35);
#2700=PRODUCT_DEFINITION_SHAPE($,$,#36);
#2701=PRODUCT_DEFINITION_SHAPE($,$,#37);
#2702=PRODUCT_DEFINITION_SHAPE($,$,#38);
#2703=PRODUCT_DEFINITION_SHAPE($,$,#39);
#2704=PRODUCT_DEFINITION_SHAPE($,$,#40);
#2705=PRODUCT_DEFINITION_SHAPE($,$,#41);
#2706=PRODUCT_DEFINITION_SHAPE($,$,#42);
#2707=SHAPE_REPRESENTATION('',(#1576,#1754,#1755,#1756,#1757,#1758,#1759,
#1760,#1761),#2667);
#2708=SHAPE_REPRESENTATION('',(#1577),#2668);
#2709=SHAPE_REPRESENTATION('',(#1606),#2669);
#2710=SHAPE_REPRESENTATION('',(#1639),#2670);
#2711=SHAPE_REPRESENTATION('',(#1672),#2671);
#2712=SHAPE_REPRESENTATION('',(#1705),#2672);
#2713=SHAPE_REPRESENTATION('',(#1708),#2673);
#2714=SHAPE_REPRESENTATION('',(#1711),#2674);
#2715=SHAPE_REPRESENTATION('',(#1714),#2675);
#2716=PRODUCT_DEFINITION_CONTEXT('part definition',#2745,'design');
#2717=PRODUCT_DEFINITION('BR-151','BR-151',#2726,#2716);
#2718=PRODUCT_DEFINITION('base','Base',#2727,#2716);
#2719=PRODUCT_DEFINITION('Screw_02','Screw_02',#2728,#2716);
#2720=PRODUCT_DEFINITION('Screw_01','Screw_01',#2729,#2716);
#2721=PRODUCT_DEFINITION('Screw_03','Screw_03',#2730,#2716);
#2722=PRODUCT_DEFINITION('Ball_01','Ball_01',#2731,#2716);
#2723=PRODUCT_DEFINITION('Ball_02','Ball_02',#2732,#2716);
#2724=PRODUCT_DEFINITION('Ball_03','Ball_03',#2733,#2716);
#2725=PRODUCT_DEFINITION('Top_Part','Top_part',#2734,#2716);
#2726=PRODUCT_DEFINITION_FORMATION('',$,#2747);
#2727=PRODUCT_DEFINITION_FORMATION('',$,#2748);
#2728=PRODUCT_DEFINITION_FORMATION('',$,#2749);
#2729=PRODUCT_DEFINITION_FORMATION('',$,#2750);
#2730=PRODUCT_DEFINITION_FORMATION('',$,#2751);
#2731=PRODUCT_DEFINITION_FORMATION('',$,#2752);
#2732=PRODUCT_DEFINITION_FORMATION('',$,#2753);
#2733=PRODUCT_DEFINITION_FORMATION('',$,#2754);
#2734=PRODUCT_DEFINITION_FORMATION('',$,#2755);
#2735=PRODUCT_RELATED_PRODUCT_CATEGORY('BR-151','BR-151',(#2747));
#2736=PRODUCT_RELATED_PRODUCT_CATEGORY('Base','Base',(#2748));
#2737=PRODUCT_RELATED_PRODUCT_CATEGORY('Screw_02','Screw_02',(#2749));
#2738=PRODUCT_RELATED_PRODUCT_CATEGORY('Screw_01','Screw_01',(#2750));
#2739=PRODUCT_RELATED_PRODUCT_CATEGORY('Screw_03','Screw_03',(#2751));
#2740=PRODUCT_RELATED_PRODUCT_CATEGORY('Ball_01','Ball_01',(#2752));
#2741=PRODUCT_RELATED_PRODUCT_CATEGORY('Ball_02','Ball_02',(#2753));
#2742=PRODUCT_RELATED_PRODUCT_CATEGORY('Ball_03','Ball_03',(#2754));
#2743=PRODUCT_RELATED_PRODUCT_CATEGORY('Top_part','Top_part',(#2755));
#2744=APPLICATION_PROTOCOL_DEFINITION('international standard',
'automotive_design',2009,#2745);
#2745=APPLICATION_CONTEXT(
'Core Data for Automotive Mechanical Design Process');
#2746=PRODUCT_CONTEXT('part definition',#2745,'mechanical');
#2747=PRODUCT('BR-151','BR-151',$,(#2746));
#2748=PRODUCT('base','Base',$,(#2746));
#2749=PRODUCT('Screw_02','Screw_02',$,(#2746));
#2750=PRODUCT('Screw_01','Screw_01',$,(#2746));
#2751=PRODUCT('Screw_03','Screw_03',$,(#2746));
#2752=PRODUCT('Ball_01','Ball_01',$,(#2746));
#2753=PRODUCT('Ball_02','Ball_02',$,(#2746));
#2754=PRODUCT('Ball_03','Ball_03',$,(#2746));
#2755=PRODUCT('Top_Part','Top_part',$,(#2746));
#2756=PRESENTATION_STYLE_ASSIGNMENT((#2758));
#2757=PRESENTATION_STYLE_ASSIGNMENT((#2759));
#2758=SURFACE_STYLE_USAGE(.BOTH.,#2760);
#2759=SURFACE_STYLE_USAGE(.BOTH.,#2761);
#2760=SURFACE_SIDE_STYLE('',(#2762));
#2761=SURFACE_SIDE_STYLE('',(#2763));
#2762=SURFACE_STYLE_FILL_AREA(#2764);
#2763=SURFACE_STYLE_FILL_AREA(#2765);
#2764=FILL_AREA_STYLE('Steel - Satin',(#2766));
#2765=FILL_AREA_STYLE('Opaque(203,203,203)',(#2767));
#2766=FILL_AREA_STYLE_COLOUR('Steel - Satin',#2768);
#2767=FILL_AREA_STYLE_COLOUR('Opaque(203,203,203)',#2769);
#2768=COLOUR_RGB('Steel - Satin', 0.09019608, 0.27058824, 0.51372549);
#2769=COLOUR_RGB('Opaque(203,203,203)', 0.09019608, 0.27058824, 0.51372549);
ENDSEC;
END-ISO-10303-21;
